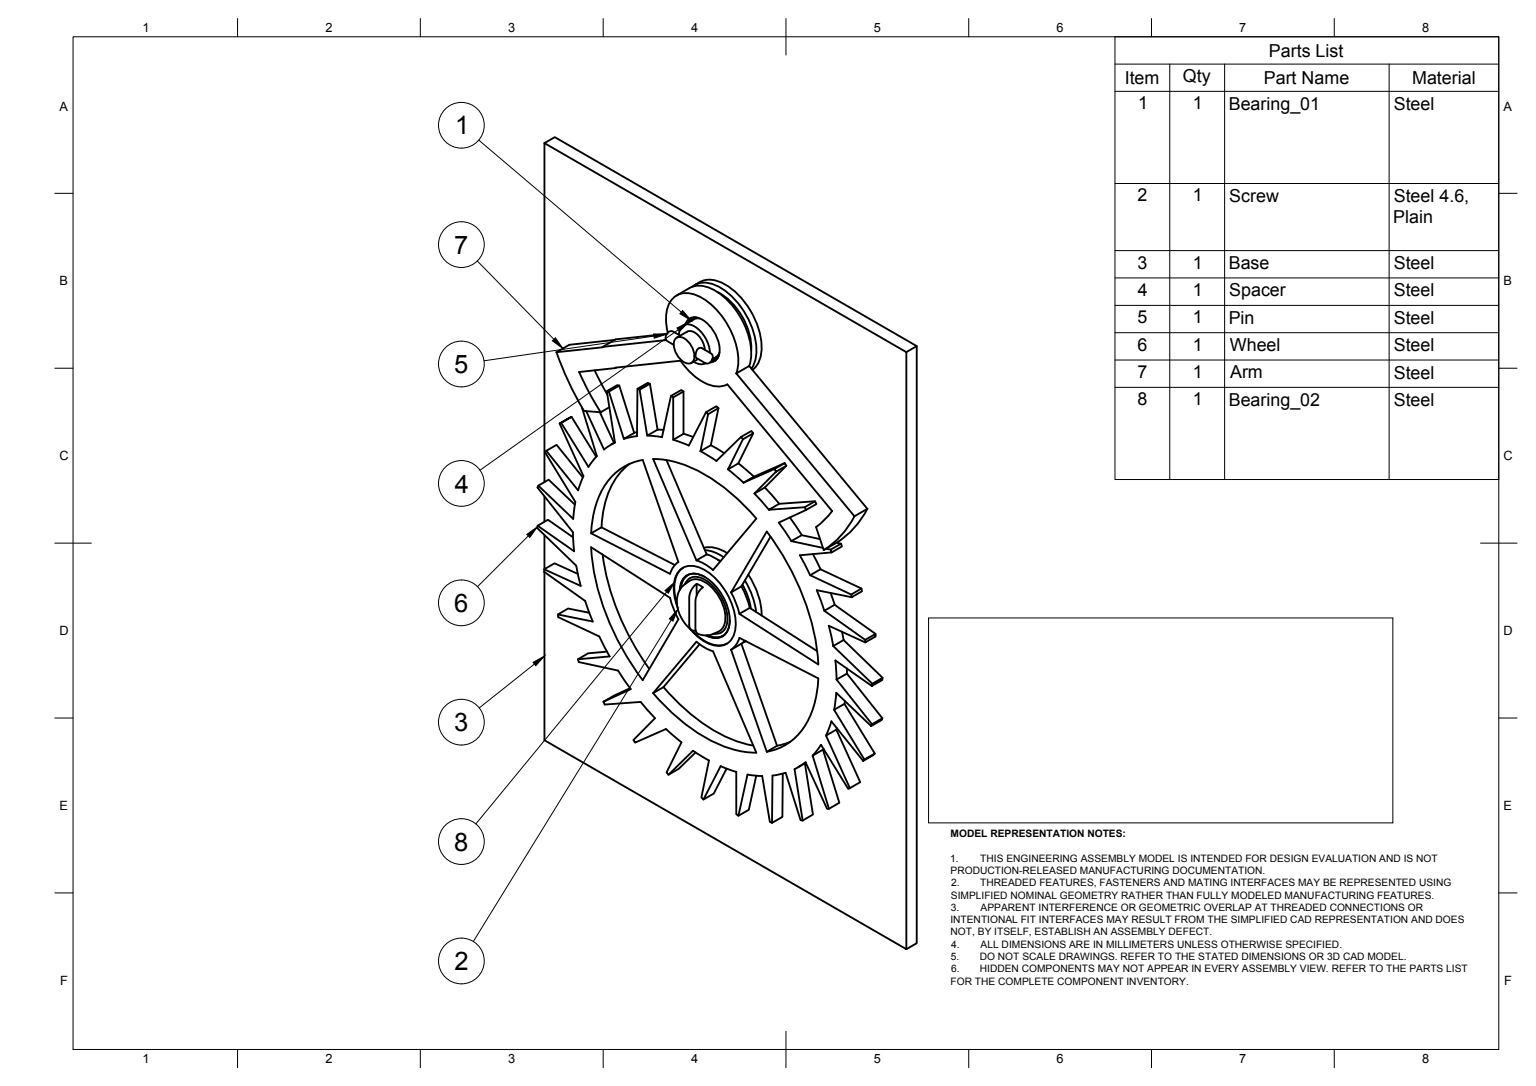
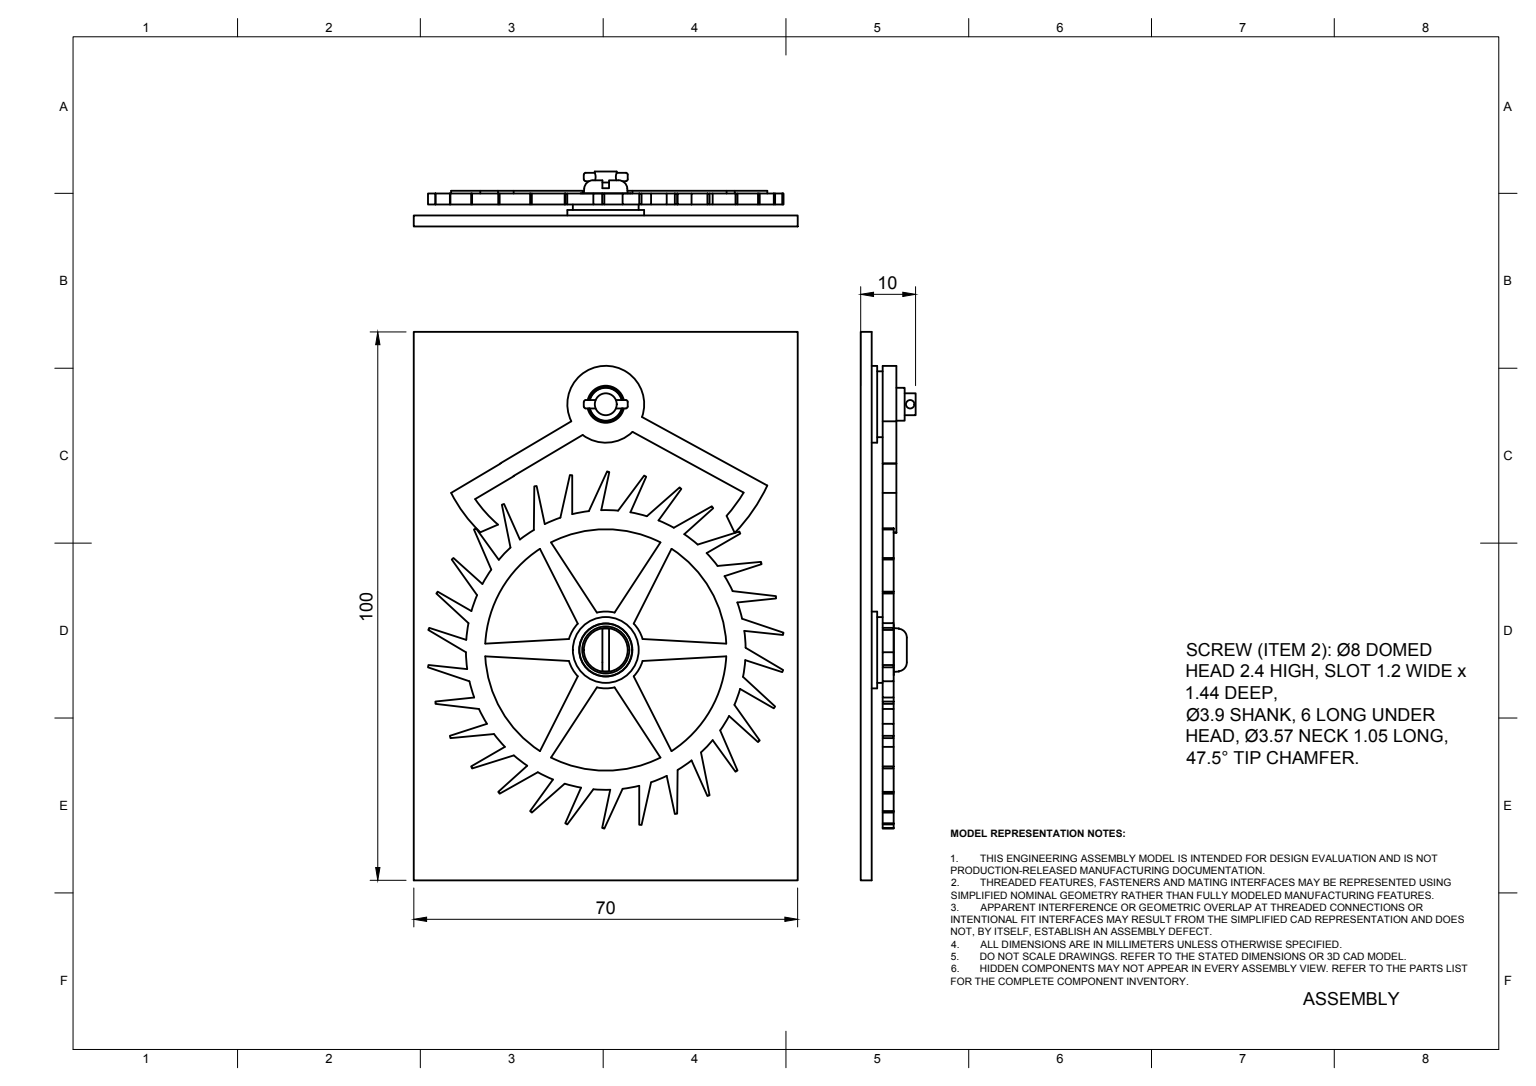
ISO-10303-21;
HEADER;
/* Generated by software containing ST-Developer
 * from STEP Tools, Inc. (www.steptools.com) 
 */

FILE_DESCRIPTION(
/* description */ (''),
/* implementation_level */ '2;1');

FILE_NAME(
/* name */ 'BR-059',
/* time_stamp */ '2026-10-04T15:18:51-07:00',
/* author */ (''),
/* organization */ (''),
/* preprocessor_version */ 'ST-DEVELOPER v20.2',
/* originating_system */ 'Autodesk Translation Framework v15.15.0.0',
/* authorisation */ '');

FILE_SCHEMA (('AUTOMOTIVE_DESIGN { 1 0 10303 214 3 1 1 }'));
ENDSEC;

DATA;
#10=MECHANICAL_DESIGN_GEOMETRIC_PRESENTATION_REPRESENTATION('',(#68,#69,
#70,#71,#72,#73,#74,#75,#76,#77,#78,#79,#80,#81),#9891);
#11=ITEM_DEFINED_TRANSFORMATION($,$,#5720,#6363);
#12=ITEM_DEFINED_TRANSFORMATION($,$,#5863,#6364);
#13=ITEM_DEFINED_TRANSFORMATION($,$,#5890,#6365);
#14=ITEM_DEFINED_TRANSFORMATION($,$,#5919,#6366);
#15=ITEM_DEFINED_TRANSFORMATION($,$,#5928,#6367);
#16=ITEM_DEFINED_TRANSFORMATION($,$,#5948,#6368);
#17=ITEM_DEFINED_TRANSFORMATION($,$,#6182,#6369);
#18=ITEM_DEFINED_TRANSFORMATION($,$,#6220,#6370);
#19=(
REPRESENTATION_RELATIONSHIP($,$,#9923,#9922)
REPRESENTATION_RELATIONSHIP_WITH_TRANSFORMATION(#11)
SHAPE_REPRESENTATION_RELATIONSHIP()
);
#20=(
REPRESENTATION_RELATIONSHIP($,$,#9924,#9922)
REPRESENTATION_RELATIONSHIP_WITH_TRANSFORMATION(#12)
SHAPE_REPRESENTATION_RELATIONSHIP()
);
#21=(
REPRESENTATION_RELATIONSHIP($,$,#9925,#9922)
REPRESENTATION_RELATIONSHIP_WITH_TRANSFORMATION(#13)
SHAPE_REPRESENTATION_RELATIONSHIP()
);
#22=(
REPRESENTATION_RELATIONSHIP($,$,#9926,#9922)
REPRESENTATION_RELATIONSHIP_WITH_TRANSFORMATION(#14)
SHAPE_REPRESENTATION_RELATIONSHIP()
);
#23=(
REPRESENTATION_RELATIONSHIP($,$,#9927,#9922)
REPRESENTATION_RELATIONSHIP_WITH_TRANSFORMATION(#15)
SHAPE_REPRESENTATION_RELATIONSHIP()
);
#24=(
REPRESENTATION_RELATIONSHIP($,$,#9928,#9922)
REPRESENTATION_RELATIONSHIP_WITH_TRANSFORMATION(#16)
SHAPE_REPRESENTATION_RELATIONSHIP()
);
#25=(
REPRESENTATION_RELATIONSHIP($,$,#9929,#9922)
REPRESENTATION_RELATIONSHIP_WITH_TRANSFORMATION(#17)
SHAPE_REPRESENTATION_RELATIONSHIP()
);
#26=(
REPRESENTATION_RELATIONSHIP($,$,#9930,#9922)
REPRESENTATION_RELATIONSHIP_WITH_TRANSFORMATION(#18)
SHAPE_REPRESENTATION_RELATIONSHIP()
);
#27=CONTEXT_DEPENDENT_SHAPE_REPRESENTATION(#19,#9914);
#28=CONTEXT_DEPENDENT_SHAPE_REPRESENTATION(#20,#9915);
#29=CONTEXT_DEPENDENT_SHAPE_REPRESENTATION(#21,#9916);
#30=CONTEXT_DEPENDENT_SHAPE_REPRESENTATION(#22,#9917);
#31=CONTEXT_DEPENDENT_SHAPE_REPRESENTATION(#23,#9918);
#32=CONTEXT_DEPENDENT_SHAPE_REPRESENTATION(#24,#9919);
#33=CONTEXT_DEPENDENT_SHAPE_REPRESENTATION(#25,#9920);
#34=CONTEXT_DEPENDENT_SHAPE_REPRESENTATION(#26,#9921);
#35=NEXT_ASSEMBLY_USAGE_OCCURRENCE('Bearing_01:1','Bearing_01:1',
'Bearing_01:1',#9932,#9933,'Bearing_01:1');
#36=NEXT_ASSEMBLY_USAGE_OCCURRENCE('Screw:1','Screw:1','Screw:1',#9932,
#9934,'Screw:1');
#37=NEXT_ASSEMBLY_USAGE_OCCURRENCE('Base:1','Base:1','Base:1',#9932,#9935,
'Base:1');
#38=NEXT_ASSEMBLY_USAGE_OCCURRENCE('Spacer:1','Spacer:1','Spacer:1',#9932,
#9936,'Spacer:1');
#39=NEXT_ASSEMBLY_USAGE_OCCURRENCE('Pin:1','Pin:1','Pin:1',#9932,#9937,
'Pin:1');
#40=NEXT_ASSEMBLY_USAGE_OCCURRENCE('Wheel:1','Wheel:1','Wheel:1',#9932,
#9938,'Wheel:1');
#41=NEXT_ASSEMBLY_USAGE_OCCURRENCE('Arm:1','Arm:1','Arm:1',#9932,#9939,
'Arm:1');
#42=NEXT_ASSEMBLY_USAGE_OCCURRENCE('Bearing_02:1','Bearing_02:1',
'Bearing_02:1',#9932,#9940,'Bearing_02:1');
#43=B_SPLINE_CURVE_WITH_KNOTS('',3,(#8377,#8378,#8379,#8380,#8381,#8382,
#8383,#8384,#8385,#8386),.UNSPECIFIED.,.F.,.F.,(4,2,2,2,4),(0.015426059292352,
0.0589123817488116,0.11818030974329,0.178151638879277,0.239555012786688),
 .UNSPECIFIED.);
#44=B_SPLINE_CURVE_WITH_KNOTS('',3,(#8390,#8391,#8392,#8393,#8394,#8395,
#8396,#8397,#8398,#8399),.UNSPECIFIED.,.F.,.F.,(4,2,2,2,4),(0.740987738910849,
0.802391112818259,0.862362441954247,0.921630369948725,0.965116692405185),
 .UNSPECIFIED.);
#45=B_SPLINE_CURVE_WITH_KNOTS('',3,(#8404,#8405,#8406,#8407,#8408,#8409,
#8410,#8411,#8412,#8413),.UNSPECIFIED.,.F.,.F.,(4,2,2,2,4),(0.740987738910849,
0.80239111281826,0.862362441954247,0.921630369948725,0.965116692405185),
 .UNSPECIFIED.);
#46=B_SPLINE_CURVE_WITH_KNOTS('',3,(#8417,#8418,#8419,#8420,#8421,#8422,
#8423,#8424,#8425,#8426),.UNSPECIFIED.,.F.,.F.,(4,2,2,2,4),(0.015426059292352,
0.0589123817488117,0.11818030974329,0.178151638879277,0.239555012786688),
 .UNSPECIFIED.);
#47=B_SPLINE_CURVE_WITH_KNOTS('',3,(#8554,#8555,#8556,#8557,#8558,#8559,
#8560,#8561,#8562,#8563,#8564,#8565,#8566,#8567,#8568,#8569,#8570,#8571,
#8572,#8573,#8574,#8575,#8576,#8577,#8578,#8579),.UNSPECIFIED.,.F.,.F.,
(4,2,2,2,2,2,2,2,2,2,2,2,4),(0.,0.0293489859798306,0.0586979719596612,0.0880217900278663,
0.117345608096071,0.146669426164276,0.175993244232481,0.205342230212312,
0.234691216192143,0.264040202171973,0.293389188151804,0.322713006220009,
0.352036824288214),.UNSPECIFIED.);
#48=B_SPLINE_CURVE_WITH_KNOTS('',3,(#8580,#8581,#8582,#8583,#8584,#8585,
#8586,#8587,#8588,#8589),.UNSPECIFIED.,.F.,.F.,(4,2,2,2,4),(0.352036824288214,
0.381360642356419,0.410684460424624,0.440033446404455,0.469382432384286),
 .UNSPECIFIED.);
#49=B_SPLINE_CURVE_WITH_KNOTS('',3,(#8602,#8603,#8604,#8605,#8606,#8607,
#8608,#8609,#8610,#8611),.UNSPECIFIED.,.F.,.F.,(4,2,2,2,4),(0.,0.0293489859798306,
0.0586979719596612,0.0880217900278663,0.117345608096071),.UNSPECIFIED.);
#50=B_SPLINE_CURVE_WITH_KNOTS('',3,(#8613,#8614,#8615,#8616,#8617,#8618,
#8619,#8620,#8621,#8622),.UNSPECIFIED.,.F.,.F.,(4,2,2,2,4),(0.352036824288214,
0.381360642356419,0.410684460424624,0.440033446404455,0.469382432384285),
 .UNSPECIFIED.);
#51=B_SPLINE_CURVE_WITH_KNOTS('',3,(#8623,#8624,#8625,#8626,#8627,#8628,
#8629,#8630,#8631,#8632,#8633,#8634,#8635,#8636,#8637,#8638,#8639,#8640),
 .UNSPECIFIED.,.F.,.F.,(4,2,2,2,2,2,2,2,4),(0.117345608096071,0.146669426164276,
0.175993244232481,0.205342230212312,0.234691216192143,0.264040202171973,
0.293389188151804,0.322713006220009,0.352036824288214),.UNSPECIFIED.);
#52=SHAPE_REPRESENTATION_RELATIONSHIP('SRR','None',#9923,#60);
#53=SHAPE_REPRESENTATION_RELATIONSHIP('SRR','None',#9924,#61);
#54=SHAPE_REPRESENTATION_RELATIONSHIP('SRR','None',#9925,#62);
#55=SHAPE_REPRESENTATION_RELATIONSHIP('SRR','None',#9926,#63);
#56=SHAPE_REPRESENTATION_RELATIONSHIP('SRR','None',#9927,#64);
#57=SHAPE_REPRESENTATION_RELATIONSHIP('SRR','None',#9928,#65);
#58=SHAPE_REPRESENTATION_RELATIONSHIP('SRR','None',#9929,#66);
#59=SHAPE_REPRESENTATION_RELATIONSHIP('SRR','None',#9930,#67);
#60=ADVANCED_BREP_SHAPE_REPRESENTATION('',(#82,#83,#84,#85),#9883);
#61=ADVANCED_BREP_SHAPE_REPRESENTATION('',(#86),#9884);
#62=ADVANCED_BREP_SHAPE_REPRESENTATION('',(#87),#9885);
#63=ADVANCED_BREP_SHAPE_REPRESENTATION('',(#88),#9886);
#64=ADVANCED_BREP_SHAPE_REPRESENTATION('',(#89),#9887);
#65=ADVANCED_BREP_SHAPE_REPRESENTATION('',(#90),#9888);
#66=ADVANCED_BREP_SHAPE_REPRESENTATION('',(#91),#9889);
#67=ADVANCED_BREP_SHAPE_REPRESENTATION('',(#92,#93,#94,#95),#9890);
#68=STYLED_ITEM('',(#9972),#82);
#69=STYLED_ITEM('',(#9972),#83);
#70=STYLED_ITEM('',(#9972),#84);
#71=STYLED_ITEM('',(#9972),#85);
#72=STYLED_ITEM('',(#9973),#86);
#73=STYLED_ITEM('',(#9974),#87);
#74=STYLED_ITEM('',(#9972),#88);
#75=STYLED_ITEM('',(#9972),#89);
#76=STYLED_ITEM('',(#9974),#90);
#77=STYLED_ITEM('',(#9975),#91);
#78=STYLED_ITEM('',(#9972),#92);
#79=STYLED_ITEM('',(#9972),#93);
#80=STYLED_ITEM('',(#9972),#94);
#81=STYLED_ITEM('',(#9972),#95);
#82=MANIFOLD_SOLID_BREP('Body1',#5616);
#83=MANIFOLD_SOLID_BREP('Body2',#5617);
#84=MANIFOLD_SOLID_BREP('Body3',#5618);
#85=MANIFOLD_SOLID_BREP('Body4',#5619);
#86=MANIFOLD_SOLID_BREP('Body1',#5620);
#87=MANIFOLD_SOLID_BREP('Body1',#5621);
#88=MANIFOLD_SOLID_BREP('Body1',#5622);
#89=MANIFOLD_SOLID_BREP('Body1',#5623);
#90=MANIFOLD_SOLID_BREP('Body1',#5624);
#91=MANIFOLD_SOLID_BREP('Body1',#5625);
#92=MANIFOLD_SOLID_BREP('Body1',#5626);
#93=MANIFOLD_SOLID_BREP('Body2',#5627);
#94=MANIFOLD_SOLID_BREP('Body3',#5628);
#95=MANIFOLD_SOLID_BREP('Body4',#5629);
#96=FACE_BOUND('',#746,.T.);
#97=FACE_BOUND('',#748,.T.);
#98=FACE_BOUND('',#750,.T.);
#99=FACE_BOUND('',#752,.T.);
#100=FACE_BOUND('',#764,.T.);
#101=FACE_BOUND('',#766,.T.);
#102=FACE_BOUND('',#768,.T.);
#103=FACE_BOUND('',#770,.T.);
#104=FACE_BOUND('',#784,.T.);
#105=FACE_BOUND('',#786,.T.);
#106=FACE_BOUND('',#788,.T.);
#107=FACE_BOUND('',#790,.T.);
#108=FACE_BOUND('',#792,.T.);
#109=FACE_BOUND('',#806,.T.);
#110=FACE_BOUND('',#808,.T.);
#111=FACE_BOUND('',#810,.T.);
#112=FACE_BOUND('',#812,.T.);
#113=FACE_BOUND('',#814,.T.);
#114=FACE_BOUND('',#825,.T.);
#115=FACE_BOUND('',#834,.T.);
#116=FACE_BOUND('',#836,.T.);
#117=FACE_BOUND('',#837,.T.);
#118=FACE_BOUND('',#841,.T.);
#119=FACE_BOUND('',#843,.T.);
#120=FACE_BOUND('',#849,.T.);
#121=FACE_BOUND('',#850,.T.);
#122=FACE_BOUND('',#852,.T.);
#123=FACE_BOUND('',#856,.T.);
#124=FACE_BOUND('',#858,.T.);
#125=FACE_BOUND('',#867,.T.);
#126=FACE_BOUND('',#1015,.T.);
#127=FACE_BOUND('',#1016,.T.);
#128=FACE_BOUND('',#1017,.T.);
#129=FACE_BOUND('',#1018,.T.);
#130=FACE_BOUND('',#1019,.T.);
#131=FACE_BOUND('',#1020,.T.);
#132=FACE_BOUND('',#1021,.T.);
#133=FACE_BOUND('',#1023,.T.);
#134=FACE_BOUND('',#1024,.T.);
#135=FACE_BOUND('',#1025,.T.);
#136=FACE_BOUND('',#1026,.T.);
#137=FACE_BOUND('',#1027,.T.);
#138=FACE_BOUND('',#1028,.T.);
#139=FACE_BOUND('',#1029,.T.);
#140=FACE_BOUND('',#1032,.T.);
#141=FACE_BOUND('',#1034,.T.);
#142=FACE_BOUND('',#1042,.T.);
#143=FACE_BOUND('',#1063,.T.);
#144=FACE_BOUND('',#1065,.T.);
#145=FACE_BOUND('',#1067,.T.);
#146=FACE_BOUND('',#1069,.T.);
#147=FACE_BOUND('',#1081,.T.);
#148=FACE_BOUND('',#1083,.T.);
#149=FACE_BOUND('',#1085,.T.);
#150=FACE_BOUND('',#1087,.T.);
#151=FACE_BOUND('',#1101,.T.);
#152=FACE_BOUND('',#1103,.T.);
#153=FACE_BOUND('',#1105,.T.);
#154=FACE_BOUND('',#1107,.T.);
#155=FACE_BOUND('',#1109,.T.);
#156=FACE_BOUND('',#1123,.T.);
#157=FACE_BOUND('',#1125,.T.);
#158=FACE_BOUND('',#1127,.T.);
#159=FACE_BOUND('',#1129,.T.);
#160=FACE_BOUND('',#1131,.T.);
#161=PLANE('',#5744);
#162=PLANE('',#5745);
#163=PLANE('',#5746);
#164=PLANE('',#5747);
#165=PLANE('',#5777);
#166=PLANE('',#5778);
#167=PLANE('',#5779);
#168=PLANE('',#5780);
#169=PLANE('',#5817);
#170=PLANE('',#5818);
#171=PLANE('',#5819);
#172=PLANE('',#5820);
#173=PLANE('',#5821);
#174=PLANE('',#5858);
#175=PLANE('',#5859);
#176=PLANE('',#5860);
#177=PLANE('',#5861);
#178=PLANE('',#5862);
#179=PLANE('',#5867);
#180=PLANE('',#5868);
#181=PLANE('',#5869);
#182=PLANE('',#5873);
#183=PLANE('',#5875);
#184=PLANE('',#5882);
#185=PLANE('',#5883);
#186=PLANE('',#5903);
#187=PLANE('',#5904);
#188=PLANE('',#5911);
#189=PLANE('',#5912);
#190=PLANE('',#5913);
#191=PLANE('',#5914);
#192=PLANE('',#5915);
#193=PLANE('',#5916);
#194=PLANE('',#5917);
#195=PLANE('',#5918);
#196=PLANE('',#5926);
#197=PLANE('',#5927);
#198=PLANE('',#5935);
#199=PLANE('',#5942);
#200=PLANE('',#5943);
#201=PLANE('',#5947);
#202=PLANE('',#5949);
#203=PLANE('',#5950);
#204=PLANE('',#5951);
#205=PLANE('',#5958);
#206=PLANE('',#5959);
#207=PLANE('',#5960);
#208=PLANE('',#5964);
#209=PLANE('',#5965);
#210=PLANE('',#5966);
#211=PLANE('',#5970);
#212=PLANE('',#5971);
#213=PLANE('',#5972);
#214=PLANE('',#5976);
#215=PLANE('',#5977);
#216=PLANE('',#5978);
#217=PLANE('',#5982);
#218=PLANE('',#5983);
#219=PLANE('',#5984);
#220=PLANE('',#5991);
#221=PLANE('',#5992);
#222=PLANE('',#5993);
#223=PLANE('',#5994);
#224=PLANE('',#5995);
#225=PLANE('',#5996);
#226=PLANE('',#6000);
#227=PLANE('',#6001);
#228=PLANE('',#6002);
#229=PLANE('',#6009);
#230=PLANE('',#6010);
#231=PLANE('',#6011);
#232=PLANE('',#6018);
#233=PLANE('',#6019);
#234=PLANE('',#6020);
#235=PLANE('',#6021);
#236=PLANE('',#6022);
#237=PLANE('',#6023);
#238=PLANE('',#6024);
#239=PLANE('',#6025);
#240=PLANE('',#6026);
#241=PLANE('',#6030);
#242=PLANE('',#6031);
#243=PLANE('',#6032);
#244=PLANE('',#6036);
#245=PLANE('',#6037);
#246=PLANE('',#6038);
#247=PLANE('',#6045);
#248=PLANE('',#6046);
#249=PLANE('',#6047);
#250=PLANE('',#6051);
#251=PLANE('',#6052);
#252=PLANE('',#6053);
#253=PLANE('',#6057);
#254=PLANE('',#6058);
#255=PLANE('',#6059);
#256=PLANE('',#6060);
#257=PLANE('',#6061);
#258=PLANE('',#6062);
#259=PLANE('',#6069);
#260=PLANE('',#6070);
#261=PLANE('',#6071);
#262=PLANE('',#6072);
#263=PLANE('',#6073);
#264=PLANE('',#6074);
#265=PLANE('',#6081);
#266=PLANE('',#6082);
#267=PLANE('',#6083);
#268=PLANE('',#6084);
#269=PLANE('',#6085);
#270=PLANE('',#6086);
#271=PLANE('',#6093);
#272=PLANE('',#6094);
#273=PLANE('',#6095);
#274=PLANE('',#6099);
#275=PLANE('',#6100);
#276=PLANE('',#6101);
#277=PLANE('',#6105);
#278=PLANE('',#6106);
#279=PLANE('',#6107);
#280=PLANE('',#6111);
#281=PLANE('',#6112);
#282=PLANE('',#6113);
#283=PLANE('',#6120);
#284=PLANE('',#6121);
#285=PLANE('',#6122);
#286=PLANE('',#6123);
#287=PLANE('',#6124);
#288=PLANE('',#6125);
#289=PLANE('',#6126);
#290=PLANE('',#6127);
#291=PLANE('',#6128);
#292=PLANE('',#6129);
#293=PLANE('',#6130);
#294=PLANE('',#6143);
#295=PLANE('',#6144);
#296=PLANE('',#6151);
#297=PLANE('',#6152);
#298=PLANE('',#6159);
#299=PLANE('',#6160);
#300=PLANE('',#6167);
#301=PLANE('',#6168);
#302=PLANE('',#6175);
#303=PLANE('',#6176);
#304=PLANE('',#6180);
#305=PLANE('',#6181);
#306=PLANE('',#6186);
#307=PLANE('',#6188);
#308=PLANE('',#6195);
#309=PLANE('',#6198);
#310=PLANE('',#6201);
#311=PLANE('',#6202);
#312=PLANE('',#6203);
#313=PLANE('',#6209);
#314=PLANE('',#6210);
#315=PLANE('',#6213);
#316=PLANE('',#6215);
#317=PLANE('',#6217);
#318=PLANE('',#6219);
#319=PLANE('',#6244);
#320=PLANE('',#6245);
#321=PLANE('',#6246);
#322=PLANE('',#6247);
#323=PLANE('',#6277);
#324=PLANE('',#6278);
#325=PLANE('',#6279);
#326=PLANE('',#6280);
#327=PLANE('',#6317);
#328=PLANE('',#6318);
#329=PLANE('',#6319);
#330=PLANE('',#6320);
#331=PLANE('',#6321);
#332=PLANE('',#6358);
#333=PLANE('',#6359);
#334=PLANE('',#6360);
#335=PLANE('',#6361);
#336=PLANE('',#6362);
#337=TOROIDAL_SURFACE('',#5733,5.8,0.2);
#338=TOROIDAL_SURFACE('',#5739,5.8,0.2);
#339=TOROIDAL_SURFACE('',#5754,3.25741379310345,0.138976293103448);
#340=TOROIDAL_SURFACE('',#5760,3.25741379310345,0.138976293103448);
#341=TOROIDAL_SURFACE('',#5768,2.2,0.2);
#342=TOROIDAL_SURFACE('',#5774,2.2,0.2);
#343=TOROIDAL_SURFACE('',#5784,4.14313829631318,0.0900000000000005);
#344=TOROIDAL_SURFACE('',#5790,4.38370090847553,0.0200000000000002);
#345=TOROIDAL_SURFACE('',#5793,4.58,0.119999999999999);
#346=TOROIDAL_SURFACE('',#5799,4.51071796769724,0.12);
#347=TOROIDAL_SURFACE('',#5802,4.51071796769724,0.22);
#348=TOROIDAL_SURFACE('',#5808,4.58,0.219999999999999);
#349=TOROIDAL_SURFACE('',#5811,4.38370090847553,0.12);
#350=TOROIDAL_SURFACE('',#5825,4.14313829631318,0.0900000000000005);
#351=TOROIDAL_SURFACE('',#5831,4.38370090847553,0.0200000000000002);
#352=TOROIDAL_SURFACE('',#5834,4.58,0.119999999999999);
#353=TOROIDAL_SURFACE('',#5840,4.51071796769724,0.12);
#354=TOROIDAL_SURFACE('',#5843,4.51071796769724,0.22);
#355=TOROIDAL_SURFACE('',#5849,4.58,0.219999999999999);
#356=TOROIDAL_SURFACE('',#5852,4.38370090847553,0.12);
#357=TOROIDAL_SURFACE('',#5877,2.32389732910985,1.6);
#358=TOROIDAL_SURFACE('',#5929,0.420000000000005,0.35);
#359=TOROIDAL_SURFACE('',#5936,0.420000000000005,0.35);
#360=TOROIDAL_SURFACE('',#6233,5.8,0.2);
#361=TOROIDAL_SURFACE('',#6239,5.8,0.2);
#362=TOROIDAL_SURFACE('',#6254,3.25741379310345,0.138976293103448);
#363=TOROIDAL_SURFACE('',#6260,3.25741379310345,0.138976293103448);
#364=TOROIDAL_SURFACE('',#6268,2.2,0.2);
#365=TOROIDAL_SURFACE('',#6274,2.2,0.2);
#366=TOROIDAL_SURFACE('',#6284,4.14313829631318,0.0900000000000005);
#367=TOROIDAL_SURFACE('',#6290,4.38370090847553,0.0200000000000002);
#368=TOROIDAL_SURFACE('',#6293,4.58,0.119999999999999);
#369=TOROIDAL_SURFACE('',#6299,4.51071796769724,0.12);
#370=TOROIDAL_SURFACE('',#6302,4.51071796769724,0.22);
#371=TOROIDAL_SURFACE('',#6308,4.58,0.219999999999999);
#372=TOROIDAL_SURFACE('',#6311,4.38370090847553,0.12);
#373=TOROIDAL_SURFACE('',#6325,4.14313829631318,0.0900000000000005);
#374=TOROIDAL_SURFACE('',#6331,4.38370090847553,0.0200000000000002);
#375=TOROIDAL_SURFACE('',#6334,4.58,0.119999999999999);
#376=TOROIDAL_SURFACE('',#6340,4.51071796769724,0.12);
#377=TOROIDAL_SURFACE('',#6343,4.51071796769724,0.22);
#378=TOROIDAL_SURFACE('',#6349,4.58,0.219999999999999);
#379=TOROIDAL_SURFACE('',#6352,4.38370090847553,0.12);
#380=CONICAL_SURFACE('',#5731,4.8,0.785398163397444);
#381=CONICAL_SURFACE('',#5742,4.845,0.785398163397444);
#382=CONICAL_SURFACE('',#5748,3.1184375,0.785398163397448);
#383=CONICAL_SURFACE('',#5766,3.0734375,0.785398163397448);
#384=CONICAL_SURFACE('',#5788,4.36638040039984,0.52359877559829);
#385=CONICAL_SURFACE('',#5797,4.57071796769724,1.04719755119659);
#386=CONICAL_SURFACE('',#5806,4.62071796769724,1.04719755119659);
#387=CONICAL_SURFACE('',#5815,4.27977786002139,0.52359877559829);
#388=CONICAL_SURFACE('',#5829,4.36638040039984,0.52359877559829);
#389=CONICAL_SURFACE('',#5838,4.57071796769724,1.04719755119659);
#390=CONICAL_SURFACE('',#5847,4.62071796769724,1.04719755119659);
#391=CONICAL_SURFACE('',#5856,4.27977786002139,0.52359877559829);
#392=CONICAL_SURFACE('',#5864,1.8052925,0.829871117430571);
#393=CONICAL_SURFACE('',#5880,3.8950136037689,0.0872664625996596);
#394=CONICAL_SURFACE('',#5887,1.89262500000135,0.523598775596927);
#395=CONICAL_SURFACE('',#6231,4.8,0.785398163397444);
#396=CONICAL_SURFACE('',#6242,4.845,0.785398163397444);
#397=CONICAL_SURFACE('',#6248,3.1184375,0.785398163397448);
#398=CONICAL_SURFACE('',#6266,3.0734375,0.785398163397448);
#399=CONICAL_SURFACE('',#6288,4.36638040039984,0.52359877559829);
#400=CONICAL_SURFACE('',#6297,4.57071796769724,1.04719755119659);
#401=CONICAL_SURFACE('',#6306,4.62071796769724,1.04719755119659);
#402=CONICAL_SURFACE('',#6315,4.27977786002139,0.52359877559829);
#403=CONICAL_SURFACE('',#6329,4.36638040039984,0.52359877559829);
#404=CONICAL_SURFACE('',#6338,4.57071796769724,1.04719755119659);
#405=CONICAL_SURFACE('',#6347,4.62071796769724,1.04719755119659);
#406=CONICAL_SURFACE('',#6356,4.27977786002139,0.52359877559829);
#407=FACE_OUTER_BOUND('',#737,.T.);
#408=FACE_OUTER_BOUND('',#738,.T.);
#409=FACE_OUTER_BOUND('',#739,.T.);
#410=FACE_OUTER_BOUND('',#740,.T.);
#411=FACE_OUTER_BOUND('',#741,.T.);
#412=FACE_OUTER_BOUND('',#742,.T.);
#413=FACE_OUTER_BOUND('',#743,.T.);
#414=FACE_OUTER_BOUND('',#744,.T.);
#415=FACE_OUTER_BOUND('',#745,.T.);
#416=FACE_OUTER_BOUND('',#747,.T.);
#417=FACE_OUTER_BOUND('',#749,.T.);
#418=FACE_OUTER_BOUND('',#751,.T.);
#419=FACE_OUTER_BOUND('',#753,.T.);
#420=FACE_OUTER_BOUND('',#754,.T.);
#421=FACE_OUTER_BOUND('',#755,.T.);
#422=FACE_OUTER_BOUND('',#756,.T.);
#423=FACE_OUTER_BOUND('',#757,.T.);
#424=FACE_OUTER_BOUND('',#758,.T.);
#425=FACE_OUTER_BOUND('',#759,.T.);
#426=FACE_OUTER_BOUND('',#760,.T.);
#427=FACE_OUTER_BOUND('',#761,.T.);
#428=FACE_OUTER_BOUND('',#762,.T.);
#429=FACE_OUTER_BOUND('',#763,.T.);
#430=FACE_OUTER_BOUND('',#765,.T.);
#431=FACE_OUTER_BOUND('',#767,.T.);
#432=FACE_OUTER_BOUND('',#769,.T.);
#433=FACE_OUTER_BOUND('',#771,.T.);
#434=FACE_OUTER_BOUND('',#772,.T.);
#435=FACE_OUTER_BOUND('',#773,.T.);
#436=FACE_OUTER_BOUND('',#774,.T.);
#437=FACE_OUTER_BOUND('',#775,.T.);
#438=FACE_OUTER_BOUND('',#776,.T.);
#439=FACE_OUTER_BOUND('',#777,.T.);
#440=FACE_OUTER_BOUND('',#778,.T.);
#441=FACE_OUTER_BOUND('',#779,.T.);
#442=FACE_OUTER_BOUND('',#780,.T.);
#443=FACE_OUTER_BOUND('',#781,.T.);
#444=FACE_OUTER_BOUND('',#782,.T.);
#445=FACE_OUTER_BOUND('',#783,.T.);
#446=FACE_OUTER_BOUND('',#785,.T.);
#447=FACE_OUTER_BOUND('',#787,.T.);
#448=FACE_OUTER_BOUND('',#789,.T.);
#449=FACE_OUTER_BOUND('',#791,.T.);
#450=FACE_OUTER_BOUND('',#793,.T.);
#451=FACE_OUTER_BOUND('',#794,.T.);
#452=FACE_OUTER_BOUND('',#795,.T.);
#453=FACE_OUTER_BOUND('',#796,.T.);
#454=FACE_OUTER_BOUND('',#797,.T.);
#455=FACE_OUTER_BOUND('',#798,.T.);
#456=FACE_OUTER_BOUND('',#799,.T.);
#457=FACE_OUTER_BOUND('',#800,.T.);
#458=FACE_OUTER_BOUND('',#801,.T.);
#459=FACE_OUTER_BOUND('',#802,.T.);
#460=FACE_OUTER_BOUND('',#803,.T.);
#461=FACE_OUTER_BOUND('',#804,.T.);
#462=FACE_OUTER_BOUND('',#805,.T.);
#463=FACE_OUTER_BOUND('',#807,.T.);
#464=FACE_OUTER_BOUND('',#809,.T.);
#465=FACE_OUTER_BOUND('',#811,.T.);
#466=FACE_OUTER_BOUND('',#813,.T.);
#467=FACE_OUTER_BOUND('',#815,.T.);
#468=FACE_OUTER_BOUND('',#816,.T.);
#469=FACE_OUTER_BOUND('',#817,.T.);
#470=FACE_OUTER_BOUND('',#818,.T.);
#471=FACE_OUTER_BOUND('',#819,.T.);
#472=FACE_OUTER_BOUND('',#820,.T.);
#473=FACE_OUTER_BOUND('',#821,.T.);
#474=FACE_OUTER_BOUND('',#822,.T.);
#475=FACE_OUTER_BOUND('',#823,.T.);
#476=FACE_OUTER_BOUND('',#824,.T.);
#477=FACE_OUTER_BOUND('',#826,.T.);
#478=FACE_OUTER_BOUND('',#827,.T.);
#479=FACE_OUTER_BOUND('',#828,.T.);
#480=FACE_OUTER_BOUND('',#829,.T.);
#481=FACE_OUTER_BOUND('',#830,.T.);
#482=FACE_OUTER_BOUND('',#831,.T.);
#483=FACE_OUTER_BOUND('',#832,.T.);
#484=FACE_OUTER_BOUND('',#833,.T.);
#485=FACE_OUTER_BOUND('',#835,.T.);
#486=FACE_OUTER_BOUND('',#838,.T.);
#487=FACE_OUTER_BOUND('',#839,.T.);
#488=FACE_OUTER_BOUND('',#840,.T.);
#489=FACE_OUTER_BOUND('',#842,.T.);
#490=FACE_OUTER_BOUND('',#844,.T.);
#491=FACE_OUTER_BOUND('',#845,.T.);
#492=FACE_OUTER_BOUND('',#846,.T.);
#493=FACE_OUTER_BOUND('',#847,.T.);
#494=FACE_OUTER_BOUND('',#848,.T.);
#495=FACE_OUTER_BOUND('',#851,.T.);
#496=FACE_OUTER_BOUND('',#853,.T.);
#497=FACE_OUTER_BOUND('',#854,.T.);
#498=FACE_OUTER_BOUND('',#855,.T.);
#499=FACE_OUTER_BOUND('',#857,.T.);
#500=FACE_OUTER_BOUND('',#859,.T.);
#501=FACE_OUTER_BOUND('',#860,.T.);
#502=FACE_OUTER_BOUND('',#861,.T.);
#503=FACE_OUTER_BOUND('',#862,.T.);
#504=FACE_OUTER_BOUND('',#863,.T.);
#505=FACE_OUTER_BOUND('',#864,.T.);
#506=FACE_OUTER_BOUND('',#865,.T.);
#507=FACE_OUTER_BOUND('',#866,.T.);
#508=FACE_OUTER_BOUND('',#868,.T.);
#509=FACE_OUTER_BOUND('',#869,.T.);
#510=FACE_OUTER_BOUND('',#870,.T.);
#511=FACE_OUTER_BOUND('',#871,.T.);
#512=FACE_OUTER_BOUND('',#872,.T.);
#513=FACE_OUTER_BOUND('',#873,.T.);
#514=FACE_OUTER_BOUND('',#874,.T.);
#515=FACE_OUTER_BOUND('',#875,.T.);
#516=FACE_OUTER_BOUND('',#876,.T.);
#517=FACE_OUTER_BOUND('',#877,.T.);
#518=FACE_OUTER_BOUND('',#878,.T.);
#519=FACE_OUTER_BOUND('',#879,.T.);
#520=FACE_OUTER_BOUND('',#880,.T.);
#521=FACE_OUTER_BOUND('',#881,.T.);
#522=FACE_OUTER_BOUND('',#882,.T.);
#523=FACE_OUTER_BOUND('',#883,.T.);
#524=FACE_OUTER_BOUND('',#884,.T.);
#525=FACE_OUTER_BOUND('',#885,.T.);
#526=FACE_OUTER_BOUND('',#886,.T.);
#527=FACE_OUTER_BOUND('',#887,.T.);
#528=FACE_OUTER_BOUND('',#888,.T.);
#529=FACE_OUTER_BOUND('',#889,.T.);
#530=FACE_OUTER_BOUND('',#890,.T.);
#531=FACE_OUTER_BOUND('',#891,.T.);
#532=FACE_OUTER_BOUND('',#892,.T.);
#533=FACE_OUTER_BOUND('',#893,.T.);
#534=FACE_OUTER_BOUND('',#894,.T.);
#535=FACE_OUTER_BOUND('',#895,.T.);
#536=FACE_OUTER_BOUND('',#896,.T.);
#537=FACE_OUTER_BOUND('',#897,.T.);
#538=FACE_OUTER_BOUND('',#898,.T.);
#539=FACE_OUTER_BOUND('',#899,.T.);
#540=FACE_OUTER_BOUND('',#900,.T.);
#541=FACE_OUTER_BOUND('',#901,.T.);
#542=FACE_OUTER_BOUND('',#902,.T.);
#543=FACE_OUTER_BOUND('',#903,.T.);
#544=FACE_OUTER_BOUND('',#904,.T.);
#545=FACE_OUTER_BOUND('',#905,.T.);
#546=FACE_OUTER_BOUND('',#906,.T.);
#547=FACE_OUTER_BOUND('',#907,.T.);
#548=FACE_OUTER_BOUND('',#908,.T.);
#549=FACE_OUTER_BOUND('',#909,.T.);
#550=FACE_OUTER_BOUND('',#910,.T.);
#551=FACE_OUTER_BOUND('',#911,.T.);
#552=FACE_OUTER_BOUND('',#912,.T.);
#553=FACE_OUTER_BOUND('',#913,.T.);
#554=FACE_OUTER_BOUND('',#914,.T.);
#555=FACE_OUTER_BOUND('',#915,.T.);
#556=FACE_OUTER_BOUND('',#916,.T.);
#557=FACE_OUTER_BOUND('',#917,.T.);
#558=FACE_OUTER_BOUND('',#918,.T.);
#559=FACE_OUTER_BOUND('',#919,.T.);
#560=FACE_OUTER_BOUND('',#920,.T.);
#561=FACE_OUTER_BOUND('',#921,.T.);
#562=FACE_OUTER_BOUND('',#922,.T.);
#563=FACE_OUTER_BOUND('',#923,.T.);
#564=FACE_OUTER_BOUND('',#924,.T.);
#565=FACE_OUTER_BOUND('',#925,.T.);
#566=FACE_OUTER_BOUND('',#926,.T.);
#567=FACE_OUTER_BOUND('',#927,.T.);
#568=FACE_OUTER_BOUND('',#928,.T.);
#569=FACE_OUTER_BOUND('',#929,.T.);
#570=FACE_OUTER_BOUND('',#930,.T.);
#571=FACE_OUTER_BOUND('',#931,.T.);
#572=FACE_OUTER_BOUND('',#932,.T.);
#573=FACE_OUTER_BOUND('',#933,.T.);
#574=FACE_OUTER_BOUND('',#934,.T.);
#575=FACE_OUTER_BOUND('',#935,.T.);
#576=FACE_OUTER_BOUND('',#936,.T.);
#577=FACE_OUTER_BOUND('',#937,.T.);
#578=FACE_OUTER_BOUND('',#938,.T.);
#579=FACE_OUTER_BOUND('',#939,.T.);
#580=FACE_OUTER_BOUND('',#940,.T.);
#581=FACE_OUTER_BOUND('',#941,.T.);
#582=FACE_OUTER_BOUND('',#942,.T.);
#583=FACE_OUTER_BOUND('',#943,.T.);
#584=FACE_OUTER_BOUND('',#944,.T.);
#585=FACE_OUTER_BOUND('',#945,.T.);
#586=FACE_OUTER_BOUND('',#946,.T.);
#587=FACE_OUTER_BOUND('',#947,.T.);
#588=FACE_OUTER_BOUND('',#948,.T.);
#589=FACE_OUTER_BOUND('',#949,.T.);
#590=FACE_OUTER_BOUND('',#950,.T.);
#591=FACE_OUTER_BOUND('',#951,.T.);
#592=FACE_OUTER_BOUND('',#952,.T.);
#593=FACE_OUTER_BOUND('',#953,.T.);
#594=FACE_OUTER_BOUND('',#954,.T.);
#595=FACE_OUTER_BOUND('',#955,.T.);
#596=FACE_OUTER_BOUND('',#956,.T.);
#597=FACE_OUTER_BOUND('',#957,.T.);
#598=FACE_OUTER_BOUND('',#958,.T.);
#599=FACE_OUTER_BOUND('',#959,.T.);
#600=FACE_OUTER_BOUND('',#960,.T.);
#601=FACE_OUTER_BOUND('',#961,.T.);
#602=FACE_OUTER_BOUND('',#962,.T.);
#603=FACE_OUTER_BOUND('',#963,.T.);
#604=FACE_OUTER_BOUND('',#964,.T.);
#605=FACE_OUTER_BOUND('',#965,.T.);
#606=FACE_OUTER_BOUND('',#966,.T.);
#607=FACE_OUTER_BOUND('',#967,.T.);
#608=FACE_OUTER_BOUND('',#968,.T.);
#609=FACE_OUTER_BOUND('',#969,.T.);
#610=FACE_OUTER_BOUND('',#970,.T.);
#611=FACE_OUTER_BOUND('',#971,.T.);
#612=FACE_OUTER_BOUND('',#972,.T.);
#613=FACE_OUTER_BOUND('',#973,.T.);
#614=FACE_OUTER_BOUND('',#974,.T.);
#615=FACE_OUTER_BOUND('',#975,.T.);
#616=FACE_OUTER_BOUND('',#976,.T.);
#617=FACE_OUTER_BOUND('',#977,.T.);
#618=FACE_OUTER_BOUND('',#978,.T.);
#619=FACE_OUTER_BOUND('',#979,.T.);
#620=FACE_OUTER_BOUND('',#980,.T.);
#621=FACE_OUTER_BOUND('',#981,.T.);
#622=FACE_OUTER_BOUND('',#982,.T.);
#623=FACE_OUTER_BOUND('',#983,.T.);
#624=FACE_OUTER_BOUND('',#984,.T.);
#625=FACE_OUTER_BOUND('',#985,.T.);
#626=FACE_OUTER_BOUND('',#986,.T.);
#627=FACE_OUTER_BOUND('',#987,.T.);
#628=FACE_OUTER_BOUND('',#988,.T.);
#629=FACE_OUTER_BOUND('',#989,.T.);
#630=FACE_OUTER_BOUND('',#990,.T.);
#631=FACE_OUTER_BOUND('',#991,.T.);
#632=FACE_OUTER_BOUND('',#992,.T.);
#633=FACE_OUTER_BOUND('',#993,.T.);
#634=FACE_OUTER_BOUND('',#994,.T.);
#635=FACE_OUTER_BOUND('',#995,.T.);
#636=FACE_OUTER_BOUND('',#996,.T.);
#637=FACE_OUTER_BOUND('',#997,.T.);
#638=FACE_OUTER_BOUND('',#998,.T.);
#639=FACE_OUTER_BOUND('',#999,.T.);
#640=FACE_OUTER_BOUND('',#1000,.T.);
#641=FACE_OUTER_BOUND('',#1001,.T.);
#642=FACE_OUTER_BOUND('',#1002,.T.);
#643=FACE_OUTER_BOUND('',#1003,.T.);
#644=FACE_OUTER_BOUND('',#1004,.T.);
#645=FACE_OUTER_BOUND('',#1005,.T.);
#646=FACE_OUTER_BOUND('',#1006,.T.);
#647=FACE_OUTER_BOUND('',#1007,.T.);
#648=FACE_OUTER_BOUND('',#1008,.T.);
#649=FACE_OUTER_BOUND('',#1009,.T.);
#650=FACE_OUTER_BOUND('',#1010,.T.);
#651=FACE_OUTER_BOUND('',#1011,.T.);
#652=FACE_OUTER_BOUND('',#1012,.T.);
#653=FACE_OUTER_BOUND('',#1013,.T.);
#654=FACE_OUTER_BOUND('',#1014,.T.);
#655=FACE_OUTER_BOUND('',#1022,.T.);
#656=FACE_OUTER_BOUND('',#1030,.T.);
#657=FACE_OUTER_BOUND('',#1031,.T.);
#658=FACE_OUTER_BOUND('',#1033,.T.);
#659=FACE_OUTER_BOUND('',#1035,.T.);
#660=FACE_OUTER_BOUND('',#1036,.T.);
#661=FACE_OUTER_BOUND('',#1037,.T.);
#662=FACE_OUTER_BOUND('',#1038,.T.);
#663=FACE_OUTER_BOUND('',#1039,.T.);
#664=FACE_OUTER_BOUND('',#1040,.T.);
#665=FACE_OUTER_BOUND('',#1041,.T.);
#666=FACE_OUTER_BOUND('',#1043,.T.);
#667=FACE_OUTER_BOUND('',#1044,.T.);
#668=FACE_OUTER_BOUND('',#1045,.T.);
#669=FACE_OUTER_BOUND('',#1046,.T.);
#670=FACE_OUTER_BOUND('',#1047,.T.);
#671=FACE_OUTER_BOUND('',#1048,.T.);
#672=FACE_OUTER_BOUND('',#1049,.T.);
#673=FACE_OUTER_BOUND('',#1050,.T.);
#674=FACE_OUTER_BOUND('',#1051,.T.);
#675=FACE_OUTER_BOUND('',#1052,.T.);
#676=FACE_OUTER_BOUND('',#1053,.T.);
#677=FACE_OUTER_BOUND('',#1054,.T.);
#678=FACE_OUTER_BOUND('',#1055,.T.);
#679=FACE_OUTER_BOUND('',#1056,.T.);
#680=FACE_OUTER_BOUND('',#1057,.T.);
#681=FACE_OUTER_BOUND('',#1058,.T.);
#682=FACE_OUTER_BOUND('',#1059,.T.);
#683=FACE_OUTER_BOUND('',#1060,.T.);
#684=FACE_OUTER_BOUND('',#1061,.T.);
#685=FACE_OUTER_BOUND('',#1062,.T.);
#686=FACE_OUTER_BOUND('',#1064,.T.);
#687=FACE_OUTER_BOUND('',#1066,.T.);
#688=FACE_OUTER_BOUND('',#1068,.T.);
#689=FACE_OUTER_BOUND('',#1070,.T.);
#690=FACE_OUTER_BOUND('',#1071,.T.);
#691=FACE_OUTER_BOUND('',#1072,.T.);
#692=FACE_OUTER_BOUND('',#1073,.T.);
#693=FACE_OUTER_BOUND('',#1074,.T.);
#694=FACE_OUTER_BOUND('',#1075,.T.);
#695=FACE_OUTER_BOUND('',#1076,.T.);
#696=FACE_OUTER_BOUND('',#1077,.T.);
#697=FACE_OUTER_BOUND('',#1078,.T.);
#698=FACE_OUTER_BOUND('',#1079,.T.);
#699=FACE_OUTER_BOUND('',#1080,.T.);
#700=FACE_OUTER_BOUND('',#1082,.T.);
#701=FACE_OUTER_BOUND('',#1084,.T.);
#702=FACE_OUTER_BOUND('',#1086,.T.);
#703=FACE_OUTER_BOUND('',#1088,.T.);
#704=FACE_OUTER_BOUND('',#1089,.T.);
#705=FACE_OUTER_BOUND('',#1090,.T.);
#706=FACE_OUTER_BOUND('',#1091,.T.);
#707=FACE_OUTER_BOUND('',#1092,.T.);
#708=FACE_OUTER_BOUND('',#1093,.T.);
#709=FACE_OUTER_BOUND('',#1094,.T.);
#710=FACE_OUTER_BOUND('',#1095,.T.);
#711=FACE_OUTER_BOUND('',#1096,.T.);
#712=FACE_OUTER_BOUND('',#1097,.T.);
#713=FACE_OUTER_BOUND('',#1098,.T.);
#714=FACE_OUTER_BOUND('',#1099,.T.);
#715=FACE_OUTER_BOUND('',#1100,.T.);
#716=FACE_OUTER_BOUND('',#1102,.T.);
#717=FACE_OUTER_BOUND('',#1104,.T.);
#718=FACE_OUTER_BOUND('',#1106,.T.);
#719=FACE_OUTER_BOUND('',#1108,.T.);
#720=FACE_OUTER_BOUND('',#1110,.T.);
#721=FACE_OUTER_BOUND('',#1111,.T.);
#722=FACE_OUTER_BOUND('',#1112,.T.);
#723=FACE_OUTER_BOUND('',#1113,.T.);
#724=FACE_OUTER_BOUND('',#1114,.T.);
#725=FACE_OUTER_BOUND('',#1115,.T.);
#726=FACE_OUTER_BOUND('',#1116,.T.);
#727=FACE_OUTER_BOUND('',#1117,.T.);
#728=FACE_OUTER_BOUND('',#1118,.T.);
#729=FACE_OUTER_BOUND('',#1119,.T.);
#730=FACE_OUTER_BOUND('',#1120,.T.);
#731=FACE_OUTER_BOUND('',#1121,.T.);
#732=FACE_OUTER_BOUND('',#1122,.T.);
#733=FACE_OUTER_BOUND('',#1124,.T.);
#734=FACE_OUTER_BOUND('',#1126,.T.);
#735=FACE_OUTER_BOUND('',#1128,.T.);
#736=FACE_OUTER_BOUND('',#1130,.T.);
#737=EDGE_LOOP('',(#3646,#3647,#3648,#3649));
#738=EDGE_LOOP('',(#3650,#3651,#3652,#3653));
#739=EDGE_LOOP('',(#3654,#3655,#3656,#3657,#3658));
#740=EDGE_LOOP('',(#3659,#3660,#3661,#3662,#3663));
#741=EDGE_LOOP('',(#3664,#3665,#3666,#3667));
#742=EDGE_LOOP('',(#3668,#3669,#3670,#3671));
#743=EDGE_LOOP('',(#3672,#3673,#3674,#3675));
#744=EDGE_LOOP('',(#3676,#3677,#3678,#3679));
#745=EDGE_LOOP('',(#3680));
#746=EDGE_LOOP('',(#3681));
#747=EDGE_LOOP('',(#3682));
#748=EDGE_LOOP('',(#3683));
#749=EDGE_LOOP('',(#3684));
#750=EDGE_LOOP('',(#3685));
#751=EDGE_LOOP('',(#3686));
#752=EDGE_LOOP('',(#3687));
#753=EDGE_LOOP('',(#3688,#3689,#3690,#3691,#3692));
#754=EDGE_LOOP('',(#3693,#3694,#3695,#3696,#3697));
#755=EDGE_LOOP('',(#3698,#3699,#3700,#3701));
#756=EDGE_LOOP('',(#3702,#3703,#3704,#3705));
#757=EDGE_LOOP('',(#3706,#3707,#3708,#3709));
#758=EDGE_LOOP('',(#3710,#3711,#3712,#3713));
#759=EDGE_LOOP('',(#3714,#3715,#3716,#3717));
#760=EDGE_LOOP('',(#3718,#3719,#3720,#3721));
#761=EDGE_LOOP('',(#3722,#3723,#3724,#3725));
#762=EDGE_LOOP('',(#3726,#3727,#3728,#3729));
#763=EDGE_LOOP('',(#3730));
#764=EDGE_LOOP('',(#3731));
#765=EDGE_LOOP('',(#3732));
#766=EDGE_LOOP('',(#3733));
#767=EDGE_LOOP('',(#3734));
#768=EDGE_LOOP('',(#3735));
#769=EDGE_LOOP('',(#3736));
#770=EDGE_LOOP('',(#3737));
#771=EDGE_LOOP('',(#3738,#3739,#3740,#3741));
#772=EDGE_LOOP('',(#3742,#3743,#3744,#3745));
#773=EDGE_LOOP('',(#3746,#3747,#3748,#3749));
#774=EDGE_LOOP('',(#3750,#3751,#3752,#3753));
#775=EDGE_LOOP('',(#3754,#3755,#3756,#3757));
#776=EDGE_LOOP('',(#3758,#3759,#3760,#3761));
#777=EDGE_LOOP('',(#3762,#3763,#3764,#3765));
#778=EDGE_LOOP('',(#3766,#3767,#3768,#3769));
#779=EDGE_LOOP('',(#3770,#3771,#3772,#3773));
#780=EDGE_LOOP('',(#3774,#3775,#3776,#3777));
#781=EDGE_LOOP('',(#3778,#3779,#3780,#3781));
#782=EDGE_LOOP('',(#3782,#3783,#3784,#3785));
#783=EDGE_LOOP('',(#3786));
#784=EDGE_LOOP('',(#3787));
#785=EDGE_LOOP('',(#3788));
#786=EDGE_LOOP('',(#3789));
#787=EDGE_LOOP('',(#3790));
#788=EDGE_LOOP('',(#3791));
#789=EDGE_LOOP('',(#3792));
#790=EDGE_LOOP('',(#3793));
#791=EDGE_LOOP('',(#3794));
#792=EDGE_LOOP('',(#3795));
#793=EDGE_LOOP('',(#3796,#3797,#3798,#3799));
#794=EDGE_LOOP('',(#3800,#3801,#3802,#3803));
#795=EDGE_LOOP('',(#3804,#3805,#3806,#3807));
#796=EDGE_LOOP('',(#3808,#3809,#3810,#3811));
#797=EDGE_LOOP('',(#3812,#3813,#3814,#3815));
#798=EDGE_LOOP('',(#3816,#3817,#3818,#3819));
#799=EDGE_LOOP('',(#3820,#3821,#3822,#3823));
#800=EDGE_LOOP('',(#3824,#3825,#3826,#3827));
#801=EDGE_LOOP('',(#3828,#3829,#3830,#3831));
#802=EDGE_LOOP('',(#3832,#3833,#3834,#3835));
#803=EDGE_LOOP('',(#3836,#3837,#3838,#3839));
#804=EDGE_LOOP('',(#3840,#3841,#3842,#3843));
#805=EDGE_LOOP('',(#3844));
#806=EDGE_LOOP('',(#3845));
#807=EDGE_LOOP('',(#3846));
#808=EDGE_LOOP('',(#3847));
#809=EDGE_LOOP('',(#3848));
#810=EDGE_LOOP('',(#3849));
#811=EDGE_LOOP('',(#3850));
#812=EDGE_LOOP('',(#3851));
#813=EDGE_LOOP('',(#3852));
#814=EDGE_LOOP('',(#3853));
#815=EDGE_LOOP('',(#3854,#3855,#3856,#3857));
#816=EDGE_LOOP('',(#3858,#3859,#3860,#3861));
#817=EDGE_LOOP('',(#3862,#3863,#3864,#3865));
#818=EDGE_LOOP('',(#3866,#3867,#3868,#3869,#3870));
#819=EDGE_LOOP('',(#3871,#3872));
#820=EDGE_LOOP('',(#3873,#3874));
#821=EDGE_LOOP('',(#3875,#3876,#3877,#3878,#3879,#3880,#3881,#3882,#3883,
#3884,#3885,#3886));
#822=EDGE_LOOP('',(#3887,#3888,#3889,#3890));
#823=EDGE_LOOP('',(#3891));
#824=EDGE_LOOP('',(#3892));
#825=EDGE_LOOP('',(#3893));
#826=EDGE_LOOP('',(#3894,#3895,#3896,#3897));
#827=EDGE_LOOP('',(#3898,#3899,#3900,#3901));
#828=EDGE_LOOP('',(#3902,#3903,#3904,#3905));
#829=EDGE_LOOP('',(#3906,#3907,#3908,#3909));
#830=EDGE_LOOP('',(#3910,#3911,#3912,#3913));
#831=EDGE_LOOP('',(#3914,#3915,#3916,#3917));
#832=EDGE_LOOP('',(#3918,#3919,#3920,#3921));
#833=EDGE_LOOP('',(#3922));
#834=EDGE_LOOP('',(#3923));
#835=EDGE_LOOP('',(#3924,#3925,#3926,#3927));
#836=EDGE_LOOP('',(#3928));
#837=EDGE_LOOP('',(#3929));
#838=EDGE_LOOP('',(#3930,#3931,#3932,#3933));
#839=EDGE_LOOP('',(#3934,#3935,#3936,#3937));
#840=EDGE_LOOP('',(#3938));
#841=EDGE_LOOP('',(#3939));
#842=EDGE_LOOP('',(#3940));
#843=EDGE_LOOP('',(#3941));
#844=EDGE_LOOP('',(#3942,#3943,#3944,#3945));
#845=EDGE_LOOP('',(#3946,#3947,#3948,#3949));
#846=EDGE_LOOP('',(#3950,#3951,#3952,#3953));
#847=EDGE_LOOP('',(#3954,#3955,#3956,#3957));
#848=EDGE_LOOP('',(#3958,#3959,#3960,#3961));
#849=EDGE_LOOP('',(#3962));
#850=EDGE_LOOP('',(#3963));
#851=EDGE_LOOP('',(#3964));
#852=EDGE_LOOP('',(#3965));
#853=EDGE_LOOP('',(#3966,#3967,#3968,#3969));
#854=EDGE_LOOP('',(#3970,#3971,#3972,#3973));
#855=EDGE_LOOP('',(#3974));
#856=EDGE_LOOP('',(#3975));
#857=EDGE_LOOP('',(#3976));
#858=EDGE_LOOP('',(#3977));
#859=EDGE_LOOP('',(#3978,#3979,#3980,#3981,#3982));
#860=EDGE_LOOP('',(#3983,#3984,#3985,#3986,#3987,#3988));
#861=EDGE_LOOP('',(#3989));
#862=EDGE_LOOP('',(#3990,#3991,#3992,#3993,#3994));
#863=EDGE_LOOP('',(#3995,#3996,#3997,#3998,#3999,#4000,#4001));
#864=EDGE_LOOP('',(#4002));
#865=EDGE_LOOP('',(#4003));
#866=EDGE_LOOP('',(#4004,#4005,#4006,#4007,#4008,#4009,#4010,#4011,#4012));
#867=EDGE_LOOP('',(#4013,#4014));
#868=EDGE_LOOP('',(#4015));
#869=EDGE_LOOP('',(#4016,#4017,#4018,#4019));
#870=EDGE_LOOP('',(#4020,#4021,#4022,#4023));
#871=EDGE_LOOP('',(#4024,#4025,#4026,#4027));
#872=EDGE_LOOP('',(#4028,#4029,#4030,#4031));
#873=EDGE_LOOP('',(#4032,#4033,#4034,#4035));
#874=EDGE_LOOP('',(#4036,#4037,#4038,#4039));
#875=EDGE_LOOP('',(#4040,#4041,#4042,#4043));
#876=EDGE_LOOP('',(#4044,#4045,#4046,#4047));
#877=EDGE_LOOP('',(#4048,#4049,#4050,#4051));
#878=EDGE_LOOP('',(#4052,#4053,#4054,#4055));
#879=EDGE_LOOP('',(#4056,#4057,#4058,#4059));
#880=EDGE_LOOP('',(#4060,#4061,#4062,#4063));
#881=EDGE_LOOP('',(#4064,#4065,#4066,#4067));
#882=EDGE_LOOP('',(#4068,#4069,#4070,#4071));
#883=EDGE_LOOP('',(#4072,#4073,#4074,#4075));
#884=EDGE_LOOP('',(#4076,#4077,#4078,#4079));
#885=EDGE_LOOP('',(#4080,#4081,#4082,#4083));
#886=EDGE_LOOP('',(#4084,#4085,#4086,#4087));
#887=EDGE_LOOP('',(#4088,#4089,#4090,#4091));
#888=EDGE_LOOP('',(#4092,#4093,#4094,#4095));
#889=EDGE_LOOP('',(#4096,#4097,#4098,#4099));
#890=EDGE_LOOP('',(#4100,#4101,#4102,#4103));
#891=EDGE_LOOP('',(#4104,#4105,#4106,#4107));
#892=EDGE_LOOP('',(#4108,#4109,#4110,#4111));
#893=EDGE_LOOP('',(#4112,#4113,#4114,#4115));
#894=EDGE_LOOP('',(#4116,#4117,#4118,#4119));
#895=EDGE_LOOP('',(#4120,#4121,#4122,#4123));
#896=EDGE_LOOP('',(#4124,#4125,#4126,#4127));
#897=EDGE_LOOP('',(#4128,#4129,#4130,#4131));
#898=EDGE_LOOP('',(#4132,#4133,#4134,#4135));
#899=EDGE_LOOP('',(#4136,#4137,#4138,#4139));
#900=EDGE_LOOP('',(#4140,#4141,#4142,#4143));
#901=EDGE_LOOP('',(#4144,#4145,#4146,#4147));
#902=EDGE_LOOP('',(#4148,#4149,#4150,#4151));
#903=EDGE_LOOP('',(#4152,#4153,#4154,#4155));
#904=EDGE_LOOP('',(#4156,#4157,#4158,#4159));
#905=EDGE_LOOP('',(#4160,#4161,#4162,#4163));
#906=EDGE_LOOP('',(#4164,#4165,#4166,#4167));
#907=EDGE_LOOP('',(#4168,#4169,#4170,#4171));
#908=EDGE_LOOP('',(#4172,#4173,#4174,#4175));
#909=EDGE_LOOP('',(#4176,#4177,#4178,#4179));
#910=EDGE_LOOP('',(#4180,#4181,#4182,#4183));
#911=EDGE_LOOP('',(#4184,#4185,#4186,#4187));
#912=EDGE_LOOP('',(#4188,#4189,#4190,#4191));
#913=EDGE_LOOP('',(#4192,#4193,#4194,#4195));
#914=EDGE_LOOP('',(#4196,#4197,#4198,#4199));
#915=EDGE_LOOP('',(#4200,#4201,#4202,#4203));
#916=EDGE_LOOP('',(#4204,#4205,#4206,#4207));
#917=EDGE_LOOP('',(#4208,#4209,#4210,#4211));
#918=EDGE_LOOP('',(#4212,#4213,#4214,#4215));
#919=EDGE_LOOP('',(#4216,#4217,#4218,#4219));
#920=EDGE_LOOP('',(#4220,#4221,#4222,#4223));
#921=EDGE_LOOP('',(#4224,#4225,#4226,#4227));
#922=EDGE_LOOP('',(#4228,#4229,#4230,#4231));
#923=EDGE_LOOP('',(#4232,#4233,#4234,#4235));
#924=EDGE_LOOP('',(#4236,#4237,#4238,#4239));
#925=EDGE_LOOP('',(#4240,#4241,#4242,#4243));
#926=EDGE_LOOP('',(#4244,#4245,#4246,#4247));
#927=EDGE_LOOP('',(#4248,#4249,#4250,#4251));
#928=EDGE_LOOP('',(#4252,#4253,#4254,#4255));
#929=EDGE_LOOP('',(#4256,#4257,#4258,#4259));
#930=EDGE_LOOP('',(#4260,#4261,#4262,#4263));
#931=EDGE_LOOP('',(#4264,#4265,#4266,#4267));
#932=EDGE_LOOP('',(#4268,#4269,#4270,#4271));
#933=EDGE_LOOP('',(#4272,#4273,#4274,#4275));
#934=EDGE_LOOP('',(#4276,#4277,#4278,#4279));
#935=EDGE_LOOP('',(#4280,#4281,#4282,#4283));
#936=EDGE_LOOP('',(#4284,#4285,#4286,#4287));
#937=EDGE_LOOP('',(#4288,#4289,#4290,#4291));
#938=EDGE_LOOP('',(#4292,#4293,#4294,#4295));
#939=EDGE_LOOP('',(#4296,#4297,#4298,#4299));
#940=EDGE_LOOP('',(#4300,#4301,#4302,#4303));
#941=EDGE_LOOP('',(#4304,#4305,#4306,#4307));
#942=EDGE_LOOP('',(#4308,#4309,#4310,#4311));
#943=EDGE_LOOP('',(#4312,#4313,#4314,#4315));
#944=EDGE_LOOP('',(#4316,#4317,#4318,#4319));
#945=EDGE_LOOP('',(#4320,#4321,#4322,#4323));
#946=EDGE_LOOP('',(#4324,#4325,#4326,#4327));
#947=EDGE_LOOP('',(#4328,#4329,#4330,#4331));
#948=EDGE_LOOP('',(#4332,#4333,#4334,#4335));
#949=EDGE_LOOP('',(#4336,#4337,#4338,#4339));
#950=EDGE_LOOP('',(#4340,#4341,#4342,#4343));
#951=EDGE_LOOP('',(#4344,#4345,#4346,#4347));
#952=EDGE_LOOP('',(#4348,#4349,#4350,#4351));
#953=EDGE_LOOP('',(#4352,#4353,#4354,#4355));
#954=EDGE_LOOP('',(#4356,#4357,#4358,#4359));
#955=EDGE_LOOP('',(#4360,#4361,#4362,#4363));
#956=EDGE_LOOP('',(#4364,#4365,#4366,#4367));
#957=EDGE_LOOP('',(#4368,#4369,#4370,#4371));
#958=EDGE_LOOP('',(#4372,#4373,#4374,#4375));
#959=EDGE_LOOP('',(#4376,#4377,#4378,#4379));
#960=EDGE_LOOP('',(#4380,#4381,#4382,#4383));
#961=EDGE_LOOP('',(#4384,#4385,#4386,#4387));
#962=EDGE_LOOP('',(#4388,#4389,#4390,#4391));
#963=EDGE_LOOP('',(#4392,#4393,#4394,#4395));
#964=EDGE_LOOP('',(#4396,#4397,#4398,#4399));
#965=EDGE_LOOP('',(#4400,#4401,#4402,#4403));
#966=EDGE_LOOP('',(#4404,#4405,#4406,#4407));
#967=EDGE_LOOP('',(#4408,#4409,#4410,#4411));
#968=EDGE_LOOP('',(#4412,#4413,#4414,#4415));
#969=EDGE_LOOP('',(#4416,#4417,#4418,#4419));
#970=EDGE_LOOP('',(#4420,#4421,#4422,#4423));
#971=EDGE_LOOP('',(#4424,#4425,#4426,#4427));
#972=EDGE_LOOP('',(#4428,#4429,#4430,#4431));
#973=EDGE_LOOP('',(#4432,#4433,#4434,#4435));
#974=EDGE_LOOP('',(#4436,#4437,#4438,#4439));
#975=EDGE_LOOP('',(#4440,#4441,#4442,#4443));
#976=EDGE_LOOP('',(#4444,#4445,#4446,#4447));
#977=EDGE_LOOP('',(#4448,#4449,#4450,#4451));
#978=EDGE_LOOP('',(#4452,#4453,#4454,#4455));
#979=EDGE_LOOP('',(#4456,#4457,#4458,#4459));
#980=EDGE_LOOP('',(#4460,#4461,#4462,#4463));
#981=EDGE_LOOP('',(#4464,#4465,#4466,#4467));
#982=EDGE_LOOP('',(#4468,#4469,#4470,#4471));
#983=EDGE_LOOP('',(#4472,#4473,#4474,#4475));
#984=EDGE_LOOP('',(#4476,#4477,#4478,#4479));
#985=EDGE_LOOP('',(#4480,#4481,#4482,#4483));
#986=EDGE_LOOP('',(#4484,#4485,#4486,#4487));
#987=EDGE_LOOP('',(#4488,#4489,#4490,#4491));
#988=EDGE_LOOP('',(#4492,#4493,#4494,#4495));
#989=EDGE_LOOP('',(#4496,#4497,#4498,#4499));
#990=EDGE_LOOP('',(#4500,#4501,#4502,#4503));
#991=EDGE_LOOP('',(#4504,#4505,#4506,#4507));
#992=EDGE_LOOP('',(#4508,#4509,#4510,#4511));
#993=EDGE_LOOP('',(#4512,#4513,#4514,#4515));
#994=EDGE_LOOP('',(#4516,#4517,#4518,#4519));
#995=EDGE_LOOP('',(#4520,#4521,#4522,#4523));
#996=EDGE_LOOP('',(#4524,#4525,#4526,#4527));
#997=EDGE_LOOP('',(#4528,#4529,#4530,#4531));
#998=EDGE_LOOP('',(#4532,#4533,#4534,#4535));
#999=EDGE_LOOP('',(#4536,#4537,#4538,#4539));
#1000=EDGE_LOOP('',(#4540,#4541,#4542,#4543));
#1001=EDGE_LOOP('',(#4544,#4545,#4546,#4547));
#1002=EDGE_LOOP('',(#4548,#4549,#4550,#4551));
#1003=EDGE_LOOP('',(#4552,#4553,#4554,#4555));
#1004=EDGE_LOOP('',(#4556,#4557,#4558,#4559));
#1005=EDGE_LOOP('',(#4560,#4561,#4562,#4563));
#1006=EDGE_LOOP('',(#4564,#4565,#4566,#4567));
#1007=EDGE_LOOP('',(#4568,#4569,#4570,#4571));
#1008=EDGE_LOOP('',(#4572,#4573,#4574,#4575));
#1009=EDGE_LOOP('',(#4576,#4577,#4578,#4579));
#1010=EDGE_LOOP('',(#4580,#4581,#4582,#4583));
#1011=EDGE_LOOP('',(#4584,#4585,#4586,#4587));
#1012=EDGE_LOOP('',(#4588,#4589,#4590,#4591));
#1013=EDGE_LOOP('',(#4592,#4593,#4594,#4595));
#1014=EDGE_LOOP('',(#4596,#4597,#4598,#4599,#4600,#4601,#4602,#4603,#4604,
#4605,#4606,#4607,#4608,#4609,#4610,#4611,#4612,#4613,#4614,#4615,#4616,
#4617,#4618,#4619,#4620,#4621,#4622,#4623,#4624,#4625,#4626,#4627,#4628,
#4629,#4630,#4631,#4632,#4633,#4634,#4635,#4636,#4637,#4638,#4639,#4640,
#4641,#4642,#4643,#4644,#4645,#4646,#4647,#4648,#4649,#4650,#4651,#4652,
#4653,#4654,#4655,#4656,#4657,#4658,#4659,#4660,#4661,#4662,#4663,#4664,
#4665,#4666,#4667,#4668,#4669,#4670,#4671,#4672,#4673,#4674,#4675,#4676,
#4677,#4678,#4679,#4680,#4681,#4682,#4683,#4684,#4685,#4686,#4687,#4688,
#4689,#4690,#4691,#4692,#4693,#4694,#4695,#4696,#4697,#4698,#4699,#4700,
#4701,#4702,#4703,#4704,#4705,#4706,#4707,#4708,#4709,#4710,#4711,#4712,
#4713,#4714,#4715));
#1015=EDGE_LOOP('',(#4716,#4717,#4718,#4719));
#1016=EDGE_LOOP('',(#4720,#4721,#4722,#4723));
#1017=EDGE_LOOP('',(#4724,#4725,#4726,#4727));
#1018=EDGE_LOOP('',(#4728,#4729,#4730,#4731));
#1019=EDGE_LOOP('',(#4732,#4733,#4734,#4735));
#1020=EDGE_LOOP('',(#4736));
#1021=EDGE_LOOP('',(#4737,#4738,#4739,#4740));
#1022=EDGE_LOOP('',(#4741,#4742,#4743,#4744,#4745,#4746,#4747,#4748,#4749,
#4750,#4751,#4752,#4753,#4754,#4755,#4756,#4757,#4758,#4759,#4760,#4761,
#4762,#4763,#4764,#4765,#4766,#4767,#4768,#4769,#4770,#4771,#4772,#4773,
#4774,#4775,#4776,#4777,#4778,#4779,#4780,#4781,#4782,#4783,#4784,#4785,
#4786,#4787,#4788,#4789,#4790,#4791,#4792,#4793,#4794,#4795,#4796,#4797,
#4798,#4799,#4800,#4801,#4802,#4803,#4804,#4805,#4806,#4807,#4808,#4809,
#4810,#4811,#4812,#4813,#4814,#4815,#4816,#4817,#4818,#4819,#4820,#4821,
#4822,#4823,#4824,#4825,#4826,#4827,#4828,#4829,#4830,#4831,#4832,#4833,
#4834,#4835,#4836,#4837,#4838,#4839,#4840,#4841,#4842,#4843,#4844,#4845,
#4846,#4847,#4848,#4849,#4850,#4851,#4852,#4853,#4854,#4855,#4856,#4857,
#4858,#4859,#4860));
#1023=EDGE_LOOP('',(#4861,#4862,#4863,#4864));
#1024=EDGE_LOOP('',(#4865,#4866,#4867,#4868));
#1025=EDGE_LOOP('',(#4869,#4870,#4871,#4872));
#1026=EDGE_LOOP('',(#4873,#4874,#4875,#4876));
#1027=EDGE_LOOP('',(#4877,#4878,#4879,#4880));
#1028=EDGE_LOOP('',(#4881));
#1029=EDGE_LOOP('',(#4882,#4883,#4884,#4885));
#1030=EDGE_LOOP('',(#4886,#4887,#4888,#4889));
#1031=EDGE_LOOP('',(#4890));
#1032=EDGE_LOOP('',(#4891));
#1033=EDGE_LOOP('',(#4892,#4893,#4894,#4895,#4896,#4897,#4898,#4899,#4900,
#4901,#4902,#4903,#4904,#4905,#4906,#4907));
#1034=EDGE_LOOP('',(#4908));
#1035=EDGE_LOOP('',(#4909,#4910,#4911,#4912));
#1036=EDGE_LOOP('',(#4913,#4914,#4915,#4916));
#1037=EDGE_LOOP('',(#4917,#4918,#4919,#4920));
#1038=EDGE_LOOP('',(#4921,#4922,#4923,#4924));
#1039=EDGE_LOOP('',(#4925,#4926,#4927,#4928));
#1040=EDGE_LOOP('',(#4929,#4930,#4931,#4932));
#1041=EDGE_LOOP('',(#4933,#4934,#4935,#4936,#4937,#4938,#4939,#4940,#4941,
#4942,#4943,#4944,#4945,#4946,#4947,#4948));
#1042=EDGE_LOOP('',(#4949));
#1043=EDGE_LOOP('',(#4950,#4951,#4952,#4953));
#1044=EDGE_LOOP('',(#4954,#4955,#4956,#4957));
#1045=EDGE_LOOP('',(#4958,#4959,#4960,#4961));
#1046=EDGE_LOOP('',(#4962,#4963,#4964,#4965));
#1047=EDGE_LOOP('',(#4966,#4967,#4968,#4969));
#1048=EDGE_LOOP('',(#4970,#4971,#4972,#4973));
#1049=EDGE_LOOP('',(#4974,#4975,#4976,#4977));
#1050=EDGE_LOOP('',(#4978,#4979,#4980,#4981));
#1051=EDGE_LOOP('',(#4982,#4983,#4984,#4985));
#1052=EDGE_LOOP('',(#4986,#4987,#4988,#4989));
#1053=EDGE_LOOP('',(#4990,#4991,#4992,#4993));
#1054=EDGE_LOOP('',(#4994,#4995,#4996,#4997));
#1055=EDGE_LOOP('',(#4998,#4999,#5000,#5001));
#1056=EDGE_LOOP('',(#5002,#5003,#5004,#5005,#5006));
#1057=EDGE_LOOP('',(#5007,#5008,#5009,#5010,#5011));
#1058=EDGE_LOOP('',(#5012,#5013,#5014,#5015));
#1059=EDGE_LOOP('',(#5016,#5017,#5018,#5019));
#1060=EDGE_LOOP('',(#5020,#5021,#5022,#5023));
#1061=EDGE_LOOP('',(#5024,#5025,#5026,#5027));
#1062=EDGE_LOOP('',(#5028));
#1063=EDGE_LOOP('',(#5029));
#1064=EDGE_LOOP('',(#5030));
#1065=EDGE_LOOP('',(#5031));
#1066=EDGE_LOOP('',(#5032));
#1067=EDGE_LOOP('',(#5033));
#1068=EDGE_LOOP('',(#5034));
#1069=EDGE_LOOP('',(#5035));
#1070=EDGE_LOOP('',(#5036,#5037,#5038,#5039,#5040));
#1071=EDGE_LOOP('',(#5041,#5042,#5043,#5044,#5045));
#1072=EDGE_LOOP('',(#5046,#5047,#5048,#5049));
#1073=EDGE_LOOP('',(#5050,#5051,#5052,#5053));
#1074=EDGE_LOOP('',(#5054,#5055,#5056,#5057));
#1075=EDGE_LOOP('',(#5058,#5059,#5060,#5061));
#1076=EDGE_LOOP('',(#5062,#5063,#5064,#5065));
#1077=EDGE_LOOP('',(#5066,#5067,#5068,#5069));
#1078=EDGE_LOOP('',(#5070,#5071,#5072,#5073));
#1079=EDGE_LOOP('',(#5074,#5075,#5076,#5077));
#1080=EDGE_LOOP('',(#5078));
#1081=EDGE_LOOP('',(#5079));
#1082=EDGE_LOOP('',(#5080));
#1083=EDGE_LOOP('',(#5081));
#1084=EDGE_LOOP('',(#5082));
#1085=EDGE_LOOP('',(#5083));
#1086=EDGE_LOOP('',(#5084));
#1087=EDGE_LOOP('',(#5085));
#1088=EDGE_LOOP('',(#5086,#5087,#5088,#5089));
#1089=EDGE_LOOP('',(#5090,#5091,#5092,#5093));
#1090=EDGE_LOOP('',(#5094,#5095,#5096,#5097));
#1091=EDGE_LOOP('',(#5098,#5099,#5100,#5101));
#1092=EDGE_LOOP('',(#5102,#5103,#5104,#5105));
#1093=EDGE_LOOP('',(#5106,#5107,#5108,#5109));
#1094=EDGE_LOOP('',(#5110,#5111,#5112,#5113));
#1095=EDGE_LOOP('',(#5114,#5115,#5116,#5117));
#1096=EDGE_LOOP('',(#5118,#5119,#5120,#5121));
#1097=EDGE_LOOP('',(#5122,#5123,#5124,#5125));
#1098=EDGE_LOOP('',(#5126,#5127,#5128,#5129));
#1099=EDGE_LOOP('',(#5130,#5131,#5132,#5133));
#1100=EDGE_LOOP('',(#5134));
#1101=EDGE_LOOP('',(#5135));
#1102=EDGE_LOOP('',(#5136));
#1103=EDGE_LOOP('',(#5137));
#1104=EDGE_LOOP('',(#5138));
#1105=EDGE_LOOP('',(#5139));
#1106=EDGE_LOOP('',(#5140));
#1107=EDGE_LOOP('',(#5141));
#1108=EDGE_LOOP('',(#5142));
#1109=EDGE_LOOP('',(#5143));
#1110=EDGE_LOOP('',(#5144,#5145,#5146,#5147));
#1111=EDGE_LOOP('',(#5148,#5149,#5150,#5151));
#1112=EDGE_LOOP('',(#5152,#5153,#5154,#5155));
#1113=EDGE_LOOP('',(#5156,#5157,#5158,#5159));
#1114=EDGE_LOOP('',(#5160,#5161,#5162,#5163));
#1115=EDGE_LOOP('',(#5164,#5165,#5166,#5167));
#1116=EDGE_LOOP('',(#5168,#5169,#5170,#5171));
#1117=EDGE_LOOP('',(#5172,#5173,#5174,#5175));
#1118=EDGE_LOOP('',(#5176,#5177,#5178,#5179));
#1119=EDGE_LOOP('',(#5180,#5181,#5182,#5183));
#1120=EDGE_LOOP('',(#5184,#5185,#5186,#5187));
#1121=EDGE_LOOP('',(#5188,#5189,#5190,#5191));
#1122=EDGE_LOOP('',(#5192));
#1123=EDGE_LOOP('',(#5193));
#1124=EDGE_LOOP('',(#5194));
#1125=EDGE_LOOP('',(#5195));
#1126=EDGE_LOOP('',(#5196));
#1127=EDGE_LOOP('',(#5197));
#1128=EDGE_LOOP('',(#5198));
#1129=EDGE_LOOP('',(#5199));
#1130=EDGE_LOOP('',(#5200));
#1131=EDGE_LOOP('',(#5201));
#1132=LINE('',#8145,#1596);
#1133=LINE('',#8151,#1597);
#1134=LINE('',#8159,#1598);
#1135=LINE('',#8163,#1599);
#1136=LINE('',#8174,#1600);
#1137=LINE('',#8181,#1601);
#1138=LINE('',#8192,#1602);
#1139=LINE('',#8197,#1603);
#1140=LINE('',#8207,#1604);
#1141=LINE('',#8217,#1605);
#1142=LINE('',#8221,#1606);
#1143=LINE('',#8231,#1607);
#1144=LINE('',#8245,#1608);
#1145=LINE('',#8256,#1609);
#1146=LINE('',#8270,#1610);
#1147=LINE('',#8284,#1611);
#1148=LINE('',#8298,#1612);
#1149=LINE('',#8308,#1613);
#1150=LINE('',#8319,#1614);
#1151=LINE('',#8333,#1615);
#1152=LINE('',#8347,#1616);
#1153=LINE('',#8361,#1617);
#1154=LINE('',#8372,#1618);
#1155=LINE('',#8388,#1619);
#1156=LINE('',#8400,#1620);
#1157=LINE('',#8415,#1621);
#1158=LINE('',#8427,#1622);
#1159=LINE('',#8444,#1623);
#1160=LINE('',#8452,#1624);
#1161=LINE('',#8456,#1625);
#1162=LINE('',#8458,#1626);
#1163=LINE('',#8464,#1627);
#1164=LINE('',#8470,#1628);
#1165=LINE('',#8476,#1629);
#1166=LINE('',#8482,#1630);
#1167=LINE('',#8488,#1631);
#1168=LINE('',#8490,#1632);
#1169=LINE('',#8492,#1633);
#1170=LINE('',#8493,#1634);
#1171=LINE('',#8500,#1635);
#1172=LINE('',#8505,#1636);
#1173=LINE('',#8510,#1637);
#1174=LINE('',#8512,#1638);
#1175=LINE('',#8513,#1639);
#1176=LINE('',#8516,#1640);
#1177=LINE('',#8517,#1641);
#1178=LINE('',#8520,#1642);
#1179=LINE('',#8521,#1643);
#1180=LINE('',#8523,#1644);
#1181=LINE('',#8531,#1645);
#1182=LINE('',#8537,#1646);
#1183=LINE('',#8552,#1647);
#1184=LINE('',#8641,#1648);
#1185=LINE('',#8649,#1649);
#1186=LINE('',#8650,#1650);
#1187=LINE('',#8656,#1651);
#1188=LINE('',#8658,#1652);
#1189=LINE('',#8660,#1653);
#1190=LINE('',#8661,#1654);
#1191=LINE('',#8664,#1655);
#1192=LINE('',#8666,#1656);
#1193=LINE('',#8667,#1657);
#1194=LINE('',#8670,#1658);
#1195=LINE('',#8672,#1659);
#1196=LINE('',#8673,#1660);
#1197=LINE('',#8678,#1661);
#1198=LINE('',#8684,#1662);
#1199=LINE('',#8689,#1663);
#1200=LINE('',#8691,#1664);
#1201=LINE('',#8693,#1665);
#1202=LINE('',#8694,#1666);
#1203=LINE('',#8697,#1667);
#1204=LINE('',#8699,#1668);
#1205=LINE('',#8700,#1669);
#1206=LINE('',#8702,#1670);
#1207=LINE('',#8703,#1671);
#1208=LINE('',#8708,#1672);
#1209=LINE('',#8713,#1673);
#1210=LINE('',#8715,#1674);
#1211=LINE('',#8717,#1675);
#1212=LINE('',#8718,#1676);
#1213=LINE('',#8721,#1677);
#1214=LINE('',#8723,#1678);
#1215=LINE('',#8724,#1679);
#1216=LINE('',#8726,#1680);
#1217=LINE('',#8727,#1681);
#1218=LINE('',#8732,#1682);
#1219=LINE('',#8737,#1683);
#1220=LINE('',#8739,#1684);
#1221=LINE('',#8741,#1685);
#1222=LINE('',#8742,#1686);
#1223=LINE('',#8745,#1687);
#1224=LINE('',#8747,#1688);
#1225=LINE('',#8748,#1689);
#1226=LINE('',#8750,#1690);
#1227=LINE('',#8751,#1691);
#1228=LINE('',#8756,#1692);
#1229=LINE('',#8761,#1693);
#1230=LINE('',#8763,#1694);
#1231=LINE('',#8765,#1695);
#1232=LINE('',#8766,#1696);
#1233=LINE('',#8769,#1697);
#1234=LINE('',#8771,#1698);
#1235=LINE('',#8772,#1699);
#1236=LINE('',#8774,#1700);
#1237=LINE('',#8775,#1701);
#1238=LINE('',#8780,#1702);
#1239=LINE('',#8785,#1703);
#1240=LINE('',#8787,#1704);
#1241=LINE('',#8789,#1705);
#1242=LINE('',#8790,#1706);
#1243=LINE('',#8793,#1707);
#1244=LINE('',#8795,#1708);
#1245=LINE('',#8796,#1709);
#1246=LINE('',#8799,#1710);
#1247=LINE('',#8801,#1711);
#1248=LINE('',#8802,#1712);
#1249=LINE('',#8807,#1713);
#1250=LINE('',#8813,#1714);
#1251=LINE('',#8818,#1715);
#1252=LINE('',#8820,#1716);
#1253=LINE('',#8822,#1717);
#1254=LINE('',#8823,#1718);
#1255=LINE('',#8825,#1719);
#1256=LINE('',#8826,#1720);
#1257=LINE('',#8828,#1721);
#1258=LINE('',#8829,#1722);
#1259=LINE('',#8833,#1723);
#1260=LINE('',#8835,#1724);
#1261=LINE('',#8837,#1725);
#1262=LINE('',#8838,#1726);
#1263=LINE('',#8841,#1727);
#1264=LINE('',#8843,#1728);
#1265=LINE('',#8844,#1729);
#1266=LINE('',#8846,#1730);
#1267=LINE('',#8847,#1731);
#1268=LINE('',#8852,#1732);
#1269=LINE('',#8857,#1733);
#1270=LINE('',#8859,#1734);
#1271=LINE('',#8861,#1735);
#1272=LINE('',#8862,#1736);
#1273=LINE('',#8865,#1737);
#1274=LINE('',#8867,#1738);
#1275=LINE('',#8868,#1739);
#1276=LINE('',#8871,#1740);
#1277=LINE('',#8873,#1741);
#1278=LINE('',#8874,#1742);
#1279=LINE('',#8879,#1743);
#1280=LINE('',#8885,#1744);
#1281=LINE('',#8890,#1745);
#1282=LINE('',#8892,#1746);
#1283=LINE('',#8894,#1747);
#1284=LINE('',#8895,#1748);
#1285=LINE('',#8898,#1749);
#1286=LINE('',#8900,#1750);
#1287=LINE('',#8901,#1751);
#1288=LINE('',#8904,#1752);
#1289=LINE('',#8906,#1753);
#1290=LINE('',#8907,#1754);
#1291=LINE('',#8912,#1755);
#1292=LINE('',#8918,#1756);
#1293=LINE('',#8923,#1757);
#1294=LINE('',#8925,#1758);
#1295=LINE('',#8927,#1759);
#1296=LINE('',#8928,#1760);
#1297=LINE('',#8930,#1761);
#1298=LINE('',#8931,#1762);
#1299=LINE('',#8933,#1763);
#1300=LINE('',#8934,#1764);
#1301=LINE('',#8938,#1765);
#1302=LINE('',#8940,#1766);
#1303=LINE('',#8942,#1767);
#1304=LINE('',#8943,#1768);
#1305=LINE('',#8945,#1769);
#1306=LINE('',#8946,#1770);
#1307=LINE('',#8948,#1771);
#1308=LINE('',#8949,#1772);
#1309=LINE('',#8953,#1773);
#1310=LINE('',#8955,#1774);
#1311=LINE('',#8957,#1775);
#1312=LINE('',#8958,#1776);
#1313=LINE('',#8961,#1777);
#1314=LINE('',#8963,#1778);
#1315=LINE('',#8964,#1779);
#1316=LINE('',#8966,#1780);
#1317=LINE('',#8967,#1781);
#1318=LINE('',#8972,#1782);
#1319=LINE('',#8977,#1783);
#1320=LINE('',#8979,#1784);
#1321=LINE('',#8981,#1785);
#1322=LINE('',#8982,#1786);
#1323=LINE('',#8985,#1787);
#1324=LINE('',#8987,#1788);
#1325=LINE('',#8988,#1789);
#1326=LINE('',#8990,#1790);
#1327=LINE('',#8991,#1791);
#1328=LINE('',#8996,#1792);
#1329=LINE('',#9001,#1793);
#1330=LINE('',#9003,#1794);
#1331=LINE('',#9005,#1795);
#1332=LINE('',#9006,#1796);
#1333=LINE('',#9009,#1797);
#1334=LINE('',#9011,#1798);
#1335=LINE('',#9012,#1799);
#1336=LINE('',#9015,#1800);
#1337=LINE('',#9017,#1801);
#1338=LINE('',#9018,#1802);
#1339=LINE('',#9023,#1803);
#1340=LINE('',#9029,#1804);
#1341=LINE('',#9034,#1805);
#1342=LINE('',#9036,#1806);
#1343=LINE('',#9038,#1807);
#1344=LINE('',#9039,#1808);
#1345=LINE('',#9042,#1809);
#1346=LINE('',#9044,#1810);
#1347=LINE('',#9045,#1811);
#1348=LINE('',#9047,#1812);
#1349=LINE('',#9048,#1813);
#1350=LINE('',#9053,#1814);
#1351=LINE('',#9058,#1815);
#1352=LINE('',#9060,#1816);
#1353=LINE('',#9062,#1817);
#1354=LINE('',#9063,#1818);
#1355=LINE('',#9066,#1819);
#1356=LINE('',#9068,#1820);
#1357=LINE('',#9069,#1821);
#1358=LINE('',#9071,#1822);
#1359=LINE('',#9072,#1823);
#1360=LINE('',#9077,#1824);
#1361=LINE('',#9082,#1825);
#1362=LINE('',#9084,#1826);
#1363=LINE('',#9086,#1827);
#1364=LINE('',#9087,#1828);
#1365=LINE('',#9089,#1829);
#1366=LINE('',#9090,#1830);
#1367=LINE('',#9092,#1831);
#1368=LINE('',#9093,#1832);
#1369=LINE('',#9097,#1833);
#1370=LINE('',#9099,#1834);
#1371=LINE('',#9101,#1835);
#1372=LINE('',#9102,#1836);
#1373=LINE('',#9105,#1837);
#1374=LINE('',#9107,#1838);
#1375=LINE('',#9108,#1839);
#1376=LINE('',#9111,#1840);
#1377=LINE('',#9113,#1841);
#1378=LINE('',#9114,#1842);
#1379=LINE('',#9119,#1843);
#1380=LINE('',#9125,#1844);
#1381=LINE('',#9130,#1845);
#1382=LINE('',#9132,#1846);
#1383=LINE('',#9134,#1847);
#1384=LINE('',#9135,#1848);
#1385=LINE('',#9137,#1849);
#1386=LINE('',#9138,#1850);
#1387=LINE('',#9140,#1851);
#1388=LINE('',#9141,#1852);
#1389=LINE('',#9145,#1853);
#1390=LINE('',#9147,#1854);
#1391=LINE('',#9149,#1855);
#1392=LINE('',#9150,#1856);
#1393=LINE('',#9153,#1857);
#1394=LINE('',#9155,#1858);
#1395=LINE('',#9156,#1859);
#1396=LINE('',#9159,#1860);
#1397=LINE('',#9161,#1861);
#1398=LINE('',#9162,#1862);
#1399=LINE('',#9167,#1863);
#1400=LINE('',#9173,#1864);
#1401=LINE('',#9178,#1865);
#1402=LINE('',#9180,#1866);
#1403=LINE('',#9182,#1867);
#1404=LINE('',#9183,#1868);
#1405=LINE('',#9185,#1869);
#1406=LINE('',#9186,#1870);
#1407=LINE('',#9188,#1871);
#1408=LINE('',#9189,#1872);
#1409=LINE('',#9193,#1873);
#1410=LINE('',#9195,#1874);
#1411=LINE('',#9197,#1875);
#1412=LINE('',#9198,#1876);
#1413=LINE('',#9201,#1877);
#1414=LINE('',#9203,#1878);
#1415=LINE('',#9204,#1879);
#1416=LINE('',#9207,#1880);
#1417=LINE('',#9209,#1881);
#1418=LINE('',#9210,#1882);
#1419=LINE('',#9215,#1883);
#1420=LINE('',#9221,#1884);
#1421=LINE('',#9226,#1885);
#1422=LINE('',#9228,#1886);
#1423=LINE('',#9230,#1887);
#1424=LINE('',#9231,#1888);
#1425=LINE('',#9234,#1889);
#1426=LINE('',#9236,#1890);
#1427=LINE('',#9237,#1891);
#1428=LINE('',#9239,#1892);
#1429=LINE('',#9240,#1893);
#1430=LINE('',#9245,#1894);
#1431=LINE('',#9250,#1895);
#1432=LINE('',#9252,#1896);
#1433=LINE('',#9254,#1897);
#1434=LINE('',#9255,#1898);
#1435=LINE('',#9258,#1899);
#1436=LINE('',#9260,#1900);
#1437=LINE('',#9261,#1901);
#1438=LINE('',#9263,#1902);
#1439=LINE('',#9264,#1903);
#1440=LINE('',#9269,#1904);
#1441=LINE('',#9274,#1905);
#1442=LINE('',#9276,#1906);
#1443=LINE('',#9278,#1907);
#1444=LINE('',#9279,#1908);
#1445=LINE('',#9281,#1909);
#1446=LINE('',#9282,#1910);
#1447=LINE('',#9285,#1911);
#1448=LINE('',#9287,#1912);
#1449=LINE('',#9288,#1913);
#1450=LINE('',#9293,#1914);
#1451=LINE('',#9298,#1915);
#1452=LINE('',#9300,#1916);
#1453=LINE('',#9302,#1917);
#1454=LINE('',#9303,#1918);
#1455=LINE('',#9306,#1919);
#1456=LINE('',#9308,#1920);
#1457=LINE('',#9309,#1921);
#1458=LINE('',#9312,#1922);
#1459=LINE('',#9314,#1923);
#1460=LINE('',#9315,#1924);
#1461=LINE('',#9320,#1925);
#1462=LINE('',#9326,#1926);
#1463=LINE('',#9331,#1927);
#1464=LINE('',#9333,#1928);
#1465=LINE('',#9335,#1929);
#1466=LINE('',#9336,#1930);
#1467=LINE('',#9338,#1931);
#1468=LINE('',#9339,#1932);
#1469=LINE('',#9341,#1933);
#1470=LINE('',#9342,#1934);
#1471=LINE('',#9346,#1935);
#1472=LINE('',#9348,#1936);
#1473=LINE('',#9350,#1937);
#1474=LINE('',#9351,#1938);
#1475=LINE('',#9353,#1939);
#1476=LINE('',#9354,#1940);
#1477=LINE('',#9356,#1941);
#1478=LINE('',#9357,#1942);
#1479=LINE('',#9361,#1943);
#1480=LINE('',#9363,#1944);
#1481=LINE('',#9365,#1945);
#1482=LINE('',#9366,#1946);
#1483=LINE('',#9368,#1947);
#1484=LINE('',#9369,#1948);
#1485=LINE('',#9371,#1949);
#1486=LINE('',#9372,#1950);
#1487=LINE('',#9376,#1951);
#1488=LINE('',#9378,#1952);
#1489=LINE('',#9380,#1953);
#1490=LINE('',#9381,#1954);
#1491=LINE('',#9385,#1955);
#1492=LINE('',#9387,#1956);
#1493=LINE('',#9389,#1957);
#1494=LINE('',#9390,#1958);
#1495=LINE('',#9395,#1959);
#1496=LINE('',#9401,#1960);
#1497=LINE('',#9407,#1961);
#1498=LINE('',#9413,#1962);
#1499=LINE('',#9416,#1963);
#1500=LINE('',#9417,#1964);
#1501=LINE('',#9421,#1965);
#1502=LINE('',#9423,#1966);
#1503=LINE('',#9425,#1967);
#1504=LINE('',#9426,#1968);
#1505=LINE('',#9431,#1969);
#1506=LINE('',#9437,#1970);
#1507=LINE('',#9440,#1971);
#1508=LINE('',#9441,#1972);
#1509=LINE('',#9445,#1973);
#1510=LINE('',#9447,#1974);
#1511=LINE('',#9449,#1975);
#1512=LINE('',#9450,#1976);
#1513=LINE('',#9455,#1977);
#1514=LINE('',#9461,#1978);
#1515=LINE('',#9464,#1979);
#1516=LINE('',#9465,#1980);
#1517=LINE('',#9469,#1981);
#1518=LINE('',#9471,#1982);
#1519=LINE('',#9473,#1983);
#1520=LINE('',#9474,#1984);
#1521=LINE('',#9479,#1985);
#1522=LINE('',#9485,#1986);
#1523=LINE('',#9488,#1987);
#1524=LINE('',#9489,#1988);
#1525=LINE('',#9493,#1989);
#1526=LINE('',#9495,#1990);
#1527=LINE('',#9497,#1991);
#1528=LINE('',#9498,#1992);
#1529=LINE('',#9503,#1993);
#1530=LINE('',#9509,#1994);
#1531=LINE('',#9512,#1995);
#1532=LINE('',#9513,#1996);
#1533=LINE('',#9515,#1997);
#1534=LINE('',#9516,#1998);
#1535=LINE('',#9521,#1999);
#1536=LINE('',#9530,#2000);
#1537=LINE('',#9538,#2001);
#1538=LINE('',#9540,#2002);
#1539=LINE('',#9542,#2003);
#1540=LINE('',#9546,#2004);
#1541=LINE('',#9550,#2005);
#1542=LINE('',#9554,#2006);
#1543=LINE('',#9558,#2007);
#1544=LINE('',#9560,#2008);
#1545=LINE('',#9562,#2009);
#1546=LINE('',#9566,#2010);
#1547=LINE('',#9570,#2011);
#1548=LINE('',#9572,#2012);
#1549=LINE('',#9573,#2013);
#1550=LINE('',#9578,#2014);
#1551=LINE('',#9579,#2015);
#1552=LINE('',#9582,#2016);
#1553=LINE('',#9583,#2017);
#1554=LINE('',#9587,#2018);
#1555=LINE('',#9590,#2019);
#1556=LINE('',#9591,#2020);
#1557=LINE('',#9593,#2021);
#1558=LINE('',#9596,#2022);
#1559=LINE('',#9598,#2023);
#1560=LINE('',#9602,#2024);
#1561=LINE('',#9606,#2025);
#1562=LINE('',#9610,#2026);
#1563=LINE('',#9613,#2027);
#1564=LINE('',#9617,#2028);
#1565=LINE('',#9619,#2029);
#1566=LINE('',#9621,#2030);
#1567=LINE('',#9623,#2031);
#1568=LINE('',#9625,#2032);
#1569=LINE('',#9627,#2033);
#1570=LINE('',#9629,#2034);
#1571=LINE('',#9631,#2035);
#1572=LINE('',#9633,#2036);
#1573=LINE('',#9635,#2037);
#1574=LINE('',#9642,#2038);
#1575=LINE('',#9648,#2039);
#1576=LINE('',#9656,#2040);
#1577=LINE('',#9660,#2041);
#1578=LINE('',#9671,#2042);
#1579=LINE('',#9678,#2043);
#1580=LINE('',#9689,#2044);
#1581=LINE('',#9694,#2045);
#1582=LINE('',#9704,#2046);
#1583=LINE('',#9714,#2047);
#1584=LINE('',#9718,#2048);
#1585=LINE('',#9728,#2049);
#1586=LINE('',#9742,#2050);
#1587=LINE('',#9753,#2051);
#1588=LINE('',#9767,#2052);
#1589=LINE('',#9781,#2053);
#1590=LINE('',#9795,#2054);
#1591=LINE('',#9805,#2055);
#1592=LINE('',#9816,#2056);
#1593=LINE('',#9830,#2057);
#1594=LINE('',#9844,#2058);
#1595=LINE('',#9858,#2059);
#1596=VECTOR('',#6379,4.8);
#1597=VECTOR('',#6386,4.872);
#1598=VECTOR('',#6395,4.8);
#1599=VECTOR('',#6400,4.8);
#1600=VECTOR('',#6415,6.);
#1601=VECTOR('',#6424,4.845);
#1602=VECTOR('',#6439,3.1184375);
#1603=VECTOR('',#6446,3.1184375);
#1604=VECTOR('',#6459,3.272);
#1605=VECTOR('',#6472,3.1184375);
#1606=VECTOR('',#6477,3.0734375);
#1607=VECTOR('',#6490,2.);
#1608=VECTOR('',#6511,3.2);
#1609=VECTOR('',#6526,4.36638040039984);
#1610=VECTOR('',#6545,4.57071796769724);
#1611=VECTOR('',#6564,4.62071796769724);
#1612=VECTOR('',#6583,4.27977786002139);
#1613=VECTOR('',#6598,3.2);
#1614=VECTOR('',#6613,4.36638040039984);
#1615=VECTOR('',#6632,4.57071796769724);
#1616=VECTOR('',#6651,4.62071796769724);
#1617=VECTOR('',#6670,4.27977786002139);
#1618=VECTOR('',#6687,1.8052925);
#1619=VECTOR('',#6692,10.);
#1620=VECTOR('',#6693,10.);
#1621=VECTOR('',#6696,10.);
#1622=VECTOR('',#6697,10.);
#1623=VECTOR('',#6724,3.8950136037689);
#1624=VECTOR('',#6735,1.78525000000062);
#1625=VECTOR('',#6740,1.89262500000135);
#1626=VECTOR('',#6743,1.954);
#1627=VECTOR('',#6750,2.);
#1628=VECTOR('',#6757,2.);
#1629=VECTOR('',#6764,6.00000000000001);
#1630=VECTOR('',#6771,7.00000000000001);
#1631=VECTOR('',#6778,10.);
#1632=VECTOR('',#6779,10.);
#1633=VECTOR('',#6780,10.);
#1634=VECTOR('',#6781,10.);
#1635=VECTOR('',#6788,6.00000000000001);
#1636=VECTOR('',#6795,7.00000000000001);
#1637=VECTOR('',#6802,10.);
#1638=VECTOR('',#6803,10.);
#1639=VECTOR('',#6804,10.);
#1640=VECTOR('',#6807,10.);
#1641=VECTOR('',#6808,10.);
#1642=VECTOR('',#6811,10.);
#1643=VECTOR('',#6812,10.);
#1644=VECTOR('',#6815,10.);
#1645=VECTOR('',#6826,1.99999999999999);
#1646=VECTOR('',#6833,2.99999999999999);
#1647=VECTOR('',#6854,0.770000000000005);
#1648=VECTOR('',#6869,0.770000000000005);
#1649=VECTOR('',#6880,1.99999999999999);
#1650=VECTOR('',#6881,1.99999999999999);
#1651=VECTOR('',#6888,10.);
#1652=VECTOR('',#6889,10.);
#1653=VECTOR('',#6890,10.);
#1654=VECTOR('',#6891,10.);
#1655=VECTOR('',#6894,10.);
#1656=VECTOR('',#6895,10.);
#1657=VECTOR('',#6896,10.);
#1658=VECTOR('',#6899,10.);
#1659=VECTOR('',#6900,10.);
#1660=VECTOR('',#6901,10.);
#1661=VECTOR('',#6906,10.);
#1662=VECTOR('',#6913,10.);
#1663=VECTOR('',#6918,10.);
#1664=VECTOR('',#6919,10.);
#1665=VECTOR('',#6920,10.);
#1666=VECTOR('',#6921,10.);
#1667=VECTOR('',#6924,10.);
#1668=VECTOR('',#6925,10.);
#1669=VECTOR('',#6926,10.);
#1670=VECTOR('',#6929,10.);
#1671=VECTOR('',#6930,10.);
#1672=VECTOR('',#6935,10.);
#1673=VECTOR('',#6940,10.);
#1674=VECTOR('',#6941,10.);
#1675=VECTOR('',#6942,10.);
#1676=VECTOR('',#6943,10.);
#1677=VECTOR('',#6946,10.);
#1678=VECTOR('',#6947,10.);
#1679=VECTOR('',#6948,10.);
#1680=VECTOR('',#6951,10.);
#1681=VECTOR('',#6952,10.);
#1682=VECTOR('',#6957,10.);
#1683=VECTOR('',#6962,10.);
#1684=VECTOR('',#6963,10.);
#1685=VECTOR('',#6964,10.);
#1686=VECTOR('',#6965,10.);
#1687=VECTOR('',#6968,10.);
#1688=VECTOR('',#6969,10.);
#1689=VECTOR('',#6970,10.);
#1690=VECTOR('',#6973,10.);
#1691=VECTOR('',#6974,10.);
#1692=VECTOR('',#6979,10.);
#1693=VECTOR('',#6984,10.);
#1694=VECTOR('',#6985,10.);
#1695=VECTOR('',#6986,10.);
#1696=VECTOR('',#6987,10.);
#1697=VECTOR('',#6990,10.);
#1698=VECTOR('',#6991,10.);
#1699=VECTOR('',#6992,10.);
#1700=VECTOR('',#6995,9.99999999999999);
#1701=VECTOR('',#6996,9.99999999999999);
#1702=VECTOR('',#7001,10.);
#1703=VECTOR('',#7006,10.);
#1704=VECTOR('',#7007,10.);
#1705=VECTOR('',#7008,10.);
#1706=VECTOR('',#7009,10.);
#1707=VECTOR('',#7012,10.);
#1708=VECTOR('',#7013,10.);
#1709=VECTOR('',#7014,10.);
#1710=VECTOR('',#7017,10.);
#1711=VECTOR('',#7018,10.);
#1712=VECTOR('',#7019,10.);
#1713=VECTOR('',#7024,10.);
#1714=VECTOR('',#7031,10.);
#1715=VECTOR('',#7036,9.99999999999999);
#1716=VECTOR('',#7037,10.);
#1717=VECTOR('',#7038,9.99999999999999);
#1718=VECTOR('',#7039,10.);
#1719=VECTOR('',#7042,10.);
#1720=VECTOR('',#7043,10.);
#1721=VECTOR('',#7046,10.);
#1722=VECTOR('',#7047,10.);
#1723=VECTOR('',#7050,10.);
#1724=VECTOR('',#7051,10.);
#1725=VECTOR('',#7052,10.);
#1726=VECTOR('',#7053,10.);
#1727=VECTOR('',#7056,10.);
#1728=VECTOR('',#7057,10.);
#1729=VECTOR('',#7058,10.);
#1730=VECTOR('',#7061,10.);
#1731=VECTOR('',#7062,10.);
#1732=VECTOR('',#7067,10.);
#1733=VECTOR('',#7072,10.);
#1734=VECTOR('',#7073,10.);
#1735=VECTOR('',#7074,10.);
#1736=VECTOR('',#7075,10.);
#1737=VECTOR('',#7078,9.99999999999999);
#1738=VECTOR('',#7079,9.99999999999999);
#1739=VECTOR('',#7080,10.);
#1740=VECTOR('',#7083,10.);
#1741=VECTOR('',#7084,10.);
#1742=VECTOR('',#7085,10.);
#1743=VECTOR('',#7090,10.);
#1744=VECTOR('',#7097,10.);
#1745=VECTOR('',#7102,10.);
#1746=VECTOR('',#7103,10.);
#1747=VECTOR('',#7104,10.);
#1748=VECTOR('',#7105,10.);
#1749=VECTOR('',#7108,10.);
#1750=VECTOR('',#7109,10.);
#1751=VECTOR('',#7110,10.);
#1752=VECTOR('',#7113,9.99999999999999);
#1753=VECTOR('',#7114,10.);
#1754=VECTOR('',#7115,9.99999999999999);
#1755=VECTOR('',#7120,10.);
#1756=VECTOR('',#7127,10.);
#1757=VECTOR('',#7132,10.);
#1758=VECTOR('',#7133,10.);
#1759=VECTOR('',#7134,10.);
#1760=VECTOR('',#7135,10.);
#1761=VECTOR('',#7138,10.);
#1762=VECTOR('',#7139,10.);
#1763=VECTOR('',#7142,10.);
#1764=VECTOR('',#7143,10.);
#1765=VECTOR('',#7146,10.);
#1766=VECTOR('',#7147,10.);
#1767=VECTOR('',#7148,10.);
#1768=VECTOR('',#7149,10.);
#1769=VECTOR('',#7152,10.);
#1770=VECTOR('',#7153,10.);
#1771=VECTOR('',#7156,10.);
#1772=VECTOR('',#7157,10.);
#1773=VECTOR('',#7160,10.);
#1774=VECTOR('',#7161,10.);
#1775=VECTOR('',#7162,10.);
#1776=VECTOR('',#7163,10.);
#1777=VECTOR('',#7166,10.);
#1778=VECTOR('',#7167,10.);
#1779=VECTOR('',#7168,10.);
#1780=VECTOR('',#7171,10.);
#1781=VECTOR('',#7172,10.);
#1782=VECTOR('',#7177,10.);
#1783=VECTOR('',#7182,10.);
#1784=VECTOR('',#7183,10.);
#1785=VECTOR('',#7184,10.);
#1786=VECTOR('',#7185,10.);
#1787=VECTOR('',#7188,10.);
#1788=VECTOR('',#7189,10.);
#1789=VECTOR('',#7190,10.);
#1790=VECTOR('',#7193,10.);
#1791=VECTOR('',#7194,10.);
#1792=VECTOR('',#7199,10.);
#1793=VECTOR('',#7204,10.);
#1794=VECTOR('',#7205,10.);
#1795=VECTOR('',#7206,10.);
#1796=VECTOR('',#7207,10.);
#1797=VECTOR('',#7210,10.);
#1798=VECTOR('',#7211,10.);
#1799=VECTOR('',#7212,10.);
#1800=VECTOR('',#7215,10.);
#1801=VECTOR('',#7216,10.);
#1802=VECTOR('',#7217,10.);
#1803=VECTOR('',#7222,10.);
#1804=VECTOR('',#7229,10.);
#1805=VECTOR('',#7234,10.);
#1806=VECTOR('',#7235,10.);
#1807=VECTOR('',#7236,10.);
#1808=VECTOR('',#7237,10.);
#1809=VECTOR('',#7240,10.);
#1810=VECTOR('',#7241,10.);
#1811=VECTOR('',#7242,10.);
#1812=VECTOR('',#7245,10.);
#1813=VECTOR('',#7246,10.);
#1814=VECTOR('',#7251,10.);
#1815=VECTOR('',#7256,10.);
#1816=VECTOR('',#7257,10.);
#1817=VECTOR('',#7258,10.);
#1818=VECTOR('',#7259,10.);
#1819=VECTOR('',#7262,10.);
#1820=VECTOR('',#7263,10.);
#1821=VECTOR('',#7264,10.);
#1822=VECTOR('',#7267,10.);
#1823=VECTOR('',#7268,10.);
#1824=VECTOR('',#7273,10.);
#1825=VECTOR('',#7278,10.);
#1826=VECTOR('',#7279,10.);
#1827=VECTOR('',#7280,10.);
#1828=VECTOR('',#7281,10.);
#1829=VECTOR('',#7284,10.);
#1830=VECTOR('',#7285,10.);
#1831=VECTOR('',#7288,10.);
#1832=VECTOR('',#7289,10.);
#1833=VECTOR('',#7292,10.);
#1834=VECTOR('',#7293,10.);
#1835=VECTOR('',#7294,10.);
#1836=VECTOR('',#7295,10.);
#1837=VECTOR('',#7298,10.);
#1838=VECTOR('',#7299,10.);
#1839=VECTOR('',#7300,10.);
#1840=VECTOR('',#7303,10.);
#1841=VECTOR('',#7304,10.);
#1842=VECTOR('',#7305,10.);
#1843=VECTOR('',#7310,10.);
#1844=VECTOR('',#7317,10.);
#1845=VECTOR('',#7322,10.);
#1846=VECTOR('',#7323,10.);
#1847=VECTOR('',#7324,10.);
#1848=VECTOR('',#7325,10.);
#1849=VECTOR('',#7328,10.);
#1850=VECTOR('',#7329,10.);
#1851=VECTOR('',#7332,10.);
#1852=VECTOR('',#7333,10.);
#1853=VECTOR('',#7336,10.);
#1854=VECTOR('',#7337,10.);
#1855=VECTOR('',#7338,10.);
#1856=VECTOR('',#7339,10.);
#1857=VECTOR('',#7342,10.);
#1858=VECTOR('',#7343,10.);
#1859=VECTOR('',#7344,10.);
#1860=VECTOR('',#7347,10.);
#1861=VECTOR('',#7348,10.);
#1862=VECTOR('',#7349,10.);
#1863=VECTOR('',#7354,10.);
#1864=VECTOR('',#7361,10.);
#1865=VECTOR('',#7366,10.);
#1866=VECTOR('',#7367,10.);
#1867=VECTOR('',#7368,10.);
#1868=VECTOR('',#7369,10.);
#1869=VECTOR('',#7372,10.);
#1870=VECTOR('',#7373,10.);
#1871=VECTOR('',#7376,10.);
#1872=VECTOR('',#7377,10.);
#1873=VECTOR('',#7380,10.);
#1874=VECTOR('',#7381,10.);
#1875=VECTOR('',#7382,10.);
#1876=VECTOR('',#7383,10.);
#1877=VECTOR('',#7386,10.);
#1878=VECTOR('',#7387,10.);
#1879=VECTOR('',#7388,10.);
#1880=VECTOR('',#7391,10.);
#1881=VECTOR('',#7392,10.);
#1882=VECTOR('',#7393,10.);
#1883=VECTOR('',#7398,10.);
#1884=VECTOR('',#7405,10.);
#1885=VECTOR('',#7410,10.);
#1886=VECTOR('',#7411,10.);
#1887=VECTOR('',#7412,10.);
#1888=VECTOR('',#7413,10.);
#1889=VECTOR('',#7416,10.);
#1890=VECTOR('',#7417,10.);
#1891=VECTOR('',#7418,10.);
#1892=VECTOR('',#7421,10.);
#1893=VECTOR('',#7422,10.);
#1894=VECTOR('',#7427,10.);
#1895=VECTOR('',#7432,10.);
#1896=VECTOR('',#7433,10.);
#1897=VECTOR('',#7434,10.);
#1898=VECTOR('',#7435,10.);
#1899=VECTOR('',#7438,10.);
#1900=VECTOR('',#7439,10.);
#1901=VECTOR('',#7440,10.);
#1902=VECTOR('',#7443,10.);
#1903=VECTOR('',#7444,10.);
#1904=VECTOR('',#7449,10.);
#1905=VECTOR('',#7454,10.);
#1906=VECTOR('',#7455,10.);
#1907=VECTOR('',#7456,10.);
#1908=VECTOR('',#7457,10.);
#1909=VECTOR('',#7460,10.);
#1910=VECTOR('',#7461,10.);
#1911=VECTOR('',#7464,10.);
#1912=VECTOR('',#7465,10.);
#1913=VECTOR('',#7466,10.);
#1914=VECTOR('',#7471,10.);
#1915=VECTOR('',#7476,10.);
#1916=VECTOR('',#7477,10.);
#1917=VECTOR('',#7478,10.);
#1918=VECTOR('',#7479,10.);
#1919=VECTOR('',#7482,10.);
#1920=VECTOR('',#7483,10.);
#1921=VECTOR('',#7484,10.);
#1922=VECTOR('',#7487,10.);
#1923=VECTOR('',#7488,10.);
#1924=VECTOR('',#7489,10.);
#1925=VECTOR('',#7494,10.);
#1926=VECTOR('',#7501,10.);
#1927=VECTOR('',#7506,10.);
#1928=VECTOR('',#7507,10.);
#1929=VECTOR('',#7508,10.);
#1930=VECTOR('',#7509,10.);
#1931=VECTOR('',#7512,10.);
#1932=VECTOR('',#7513,10.);
#1933=VECTOR('',#7516,10.);
#1934=VECTOR('',#7517,10.);
#1935=VECTOR('',#7520,10.);
#1936=VECTOR('',#7521,10.);
#1937=VECTOR('',#7522,10.);
#1938=VECTOR('',#7523,10.);
#1939=VECTOR('',#7526,10.);
#1940=VECTOR('',#7527,10.);
#1941=VECTOR('',#7530,10.);
#1942=VECTOR('',#7531,10.);
#1943=VECTOR('',#7534,10.);
#1944=VECTOR('',#7535,10.);
#1945=VECTOR('',#7536,10.);
#1946=VECTOR('',#7537,10.);
#1947=VECTOR('',#7540,10.);
#1948=VECTOR('',#7541,10.);
#1949=VECTOR('',#7544,10.);
#1950=VECTOR('',#7545,10.);
#1951=VECTOR('',#7548,10.);
#1952=VECTOR('',#7549,10.);
#1953=VECTOR('',#7550,10.);
#1954=VECTOR('',#7551,10.);
#1955=VECTOR('',#7554,10.);
#1956=VECTOR('',#7555,10.);
#1957=VECTOR('',#7556,10.);
#1958=VECTOR('',#7557,10.);
#1959=VECTOR('',#7562,10.);
#1960=VECTOR('',#7569,10.);
#1961=VECTOR('',#7576,10.);
#1962=VECTOR('',#7583,10.);
#1963=VECTOR('',#7588,10.);
#1964=VECTOR('',#7589,10.);
#1965=VECTOR('',#7592,10.);
#1966=VECTOR('',#7593,10.);
#1967=VECTOR('',#7594,10.);
#1968=VECTOR('',#7595,10.);
#1969=VECTOR('',#7600,10.);
#1970=VECTOR('',#7607,10.);
#1971=VECTOR('',#7612,10.);
#1972=VECTOR('',#7613,10.);
#1973=VECTOR('',#7616,10.);
#1974=VECTOR('',#7617,10.);
#1975=VECTOR('',#7618,10.);
#1976=VECTOR('',#7619,10.);
#1977=VECTOR('',#7624,10.);
#1978=VECTOR('',#7631,10.);
#1979=VECTOR('',#7636,10.);
#1980=VECTOR('',#7637,10.);
#1981=VECTOR('',#7640,10.);
#1982=VECTOR('',#7641,10.);
#1983=VECTOR('',#7642,10.);
#1984=VECTOR('',#7643,10.);
#1985=VECTOR('',#7648,10.);
#1986=VECTOR('',#7655,10.);
#1987=VECTOR('',#7660,10.);
#1988=VECTOR('',#7661,10.);
#1989=VECTOR('',#7664,10.);
#1990=VECTOR('',#7665,10.);
#1991=VECTOR('',#7666,10.);
#1992=VECTOR('',#7667,10.);
#1993=VECTOR('',#7672,10.);
#1994=VECTOR('',#7679,10.);
#1995=VECTOR('',#7684,9.99999999999999);
#1996=VECTOR('',#7685,9.99999999999999);
#1997=VECTOR('',#7688,10.);
#1998=VECTOR('',#7689,10.);
#1999=VECTOR('',#7694,6.00000000000001);
#2000=VECTOR('',#7707,3.37715398312954);
#2001=VECTOR('',#7716,10.);
#2002=VECTOR('',#7717,10.);
#2003=VECTOR('',#7718,10.);
#2004=VECTOR('',#7721,10.);
#2005=VECTOR('',#7724,10.);
#2006=VECTOR('',#7727,10.);
#2007=VECTOR('',#7730,10.);
#2008=VECTOR('',#7731,10.);
#2009=VECTOR('',#7732,10.);
#2010=VECTOR('',#7735,10.);
#2011=VECTOR('',#7740,10.);
#2012=VECTOR('',#7741,10.);
#2013=VECTOR('',#7742,9.99999999999999);
#2014=VECTOR('',#7747,10.);
#2015=VECTOR('',#7748,10.);
#2016=VECTOR('',#7751,10.);
#2017=VECTOR('',#7752,10.);
#2018=VECTOR('',#7757,10.);
#2019=VECTOR('',#7760,10.);
#2020=VECTOR('',#7761,10.);
#2021=VECTOR('',#7764,10.);
#2022=VECTOR('',#7767,9.99999999999999);
#2023=VECTOR('',#7768,10.);
#2024=VECTOR('',#7771,10.);
#2025=VECTOR('',#7774,10.);
#2026=VECTOR('',#7777,10.);
#2027=VECTOR('',#7780,10.);
#2028=VECTOR('',#7785,10.);
#2029=VECTOR('',#7788,10.);
#2030=VECTOR('',#7791,6.00000000000001);
#2031=VECTOR('',#7794,10.);
#2032=VECTOR('',#7797,10.);
#2033=VECTOR('',#7800,10.);
#2034=VECTOR('',#7803,10.);
#2035=VECTOR('',#7806,10.);
#2036=VECTOR('',#7809,10.);
#2037=VECTOR('',#7812,10.);
#2038=VECTOR('',#7821,4.8);
#2039=VECTOR('',#7828,4.872);
#2040=VECTOR('',#7837,4.8);
#2041=VECTOR('',#7842,4.8);
#2042=VECTOR('',#7857,6.);
#2043=VECTOR('',#7866,4.845);
#2044=VECTOR('',#7881,3.1184375);
#2045=VECTOR('',#7888,3.1184375);
#2046=VECTOR('',#7901,3.272);
#2047=VECTOR('',#7914,3.1184375);
#2048=VECTOR('',#7919,3.0734375);
#2049=VECTOR('',#7932,2.);
#2050=VECTOR('',#7953,3.2);
#2051=VECTOR('',#7968,4.36638040039984);
#2052=VECTOR('',#7987,4.57071796769724);
#2053=VECTOR('',#8006,4.62071796769724);
#2054=VECTOR('',#8025,4.27977786002139);
#2055=VECTOR('',#8040,3.2);
#2056=VECTOR('',#8055,4.36638040039984);
#2057=VECTOR('',#8074,4.57071796769724);
#2058=VECTOR('',#8093,4.62071796769724);
#2059=VECTOR('',#8112,4.27977786002139);
#2060=CIRCLE('',#5722,4.8);
#2061=CIRCLE('',#5723,4.8);
#2062=CIRCLE('',#5725,4.872);
#2063=CIRCLE('',#5726,4.872);
#2064=CIRCLE('',#5728,4.8);
#2065=CIRCLE('',#5729,4.8);
#2066=CIRCLE('',#5730,4.8);
#2067=CIRCLE('',#5732,4.845);
#2068=CIRCLE('',#5734,6.);
#2069=CIRCLE('',#5735,0.2);
#2070=CIRCLE('',#5736,5.8);
#2071=CIRCLE('',#5738,6.);
#2072=CIRCLE('',#5740,5.8);
#2073=CIRCLE('',#5741,0.2);
#2074=CIRCLE('',#5743,4.845);
#2075=CIRCLE('',#5749,3.1184375);
#2076=CIRCLE('',#5750,3.0734375);
#2077=CIRCLE('',#5751,3.1184375);
#2078=CIRCLE('',#5753,3.1184375);
#2079=CIRCLE('',#5755,0.138976293103448);
#2080=CIRCLE('',#5756,3.2);
#2081=CIRCLE('',#5758,3.272);
#2082=CIRCLE('',#5759,3.272);
#2083=CIRCLE('',#5761,3.2);
#2084=CIRCLE('',#5762,0.138976293103448);
#2085=CIRCLE('',#5763,3.1184375);
#2086=CIRCLE('',#5765,3.1184375);
#2087=CIRCLE('',#5767,3.0734375);
#2088=CIRCLE('',#5769,2.2);
#2089=CIRCLE('',#5770,0.2);
#2090=CIRCLE('',#5771,2.);
#2091=CIRCLE('',#5773,2.);
#2092=CIRCLE('',#5775,0.2);
#2093=CIRCLE('',#5776,2.2);
#2094=CIRCLE('',#5782,3.2);
#2095=CIRCLE('',#5783,3.2);
#2096=CIRCLE('',#5785,4.22108058265378);
#2097=CIRCLE('',#5786,0.0900000000000005);
#2098=CIRCLE('',#5787,4.14313829631318);
#2099=CIRCLE('',#5789,4.36638040039984);
#2100=CIRCLE('',#5791,4.38370090847553);
#2101=CIRCLE('',#5792,0.0200000000000002);
#2102=CIRCLE('',#5794,4.64);
#2103=CIRCLE('',#5795,0.119999999999999);
#2104=CIRCLE('',#5796,4.58);
#2105=CIRCLE('',#5798,4.57071796769724);
#2106=CIRCLE('',#5800,4.39071796769724);
#2107=CIRCLE('',#5801,0.12);
#2108=CIRCLE('',#5803,4.62071796769724);
#2109=CIRCLE('',#5804,0.22);
#2110=CIRCLE('',#5805,4.29071796769724);
#2111=CIRCLE('',#5807,4.69);
#2112=CIRCLE('',#5809,4.58);
#2113=CIRCLE('',#5810,0.219999999999999);
#2114=CIRCLE('',#5812,4.27977786002139);
#2115=CIRCLE('',#5813,0.12);
#2116=CIRCLE('',#5814,4.38370090847553);
#2117=CIRCLE('',#5816,4.13736479362129);
#2118=CIRCLE('',#5823,3.2);
#2119=CIRCLE('',#5824,3.2);
#2120=CIRCLE('',#5826,4.22108058265378);
#2121=CIRCLE('',#5827,0.0900000000000005);
#2122=CIRCLE('',#5828,4.14313829631318);
#2123=CIRCLE('',#5830,4.36638040039984);
#2124=CIRCLE('',#5832,4.38370090847553);
#2125=CIRCLE('',#5833,0.0200000000000002);
#2126=CIRCLE('',#5835,4.64);
#2127=CIRCLE('',#5836,0.119999999999999);
#2128=CIRCLE('',#5837,4.58);
#2129=CIRCLE('',#5839,4.57071796769724);
#2130=CIRCLE('',#5841,4.39071796769724);
#2131=CIRCLE('',#5842,0.12);
#2132=CIRCLE('',#5844,4.62071796769724);
#2133=CIRCLE('',#5845,0.22);
#2134=CIRCLE('',#5846,4.29071796769724);
#2135=CIRCLE('',#5848,4.69);
#2136=CIRCLE('',#5850,4.58);
#2137=CIRCLE('',#5851,0.219999999999999);
#2138=CIRCLE('',#5853,4.27977786002139);
#2139=CIRCLE('',#5854,0.12);
#2140=CIRCLE('',#5855,4.38370090847553);
#2141=CIRCLE('',#5857,4.13736479362129);
#2142=CIRCLE('',#5865,1.954);
#2143=CIRCLE('',#5866,1.570585);
#2144=CIRCLE('',#5870,3.91587722848039);
#2145=CIRCLE('',#5871,3.91587722848039);
#2146=CIRCLE('',#5872,3.91587722848039);
#2147=CIRCLE('',#5874,2.32389732910985);
#2148=CIRCLE('',#5876,2.32389732910985);
#2149=CIRCLE('',#5878,3.91780884605665);
#2150=CIRCLE('',#5879,1.6);
#2151=CIRCLE('',#5881,4.);
#2152=CIRCLE('',#5884,1.78524999999977);
#2153=CIRCLE('',#5886,1.78525000000146);
#2154=CIRCLE('',#5888,1.954);
#2155=CIRCLE('',#5892,2.);
#2156=CIRCLE('',#5893,2.);
#2157=CIRCLE('',#5895,2.);
#2158=CIRCLE('',#5896,2.);
#2159=CIRCLE('',#5898,6.00000000000001);
#2160=CIRCLE('',#5899,6.00000000000001);
#2161=CIRCLE('',#5901,7.00000000000001);
#2162=CIRCLE('',#5902,7.00000000000001);
#2163=CIRCLE('',#5905,7.00000000000001);
#2164=CIRCLE('',#5907,6.00000000000001);
#2165=CIRCLE('',#5908,6.00000000000001);
#2166=CIRCLE('',#5910,7.00000000000001);
#2167=CIRCLE('',#5921,1.99999999999999);
#2168=CIRCLE('',#5922,1.99999999999999);
#2169=CIRCLE('',#5924,2.99999999999999);
#2170=CIRCLE('',#5925,2.99999999999999);
#2171=CIRCLE('',#5930,0.420000000000005);
#2172=CIRCLE('',#5931,0.35);
#2173=CIRCLE('',#5932,0.770000000000005);
#2174=CIRCLE('',#5933,0.770000000000005);
#2175=CIRCLE('',#5937,0.420000000000005);
#2176=CIRCLE('',#5938,0.35);
#2177=CIRCLE('',#5939,0.770000000000005);
#2178=CIRCLE('',#5940,0.770000000000005);
#2179=CIRCLE('',#5944,1.99999999999999);
#2180=CIRCLE('',#5946,1.99999999999999);
#2181=CIRCLE('',#5953,25.5);
#2182=CIRCLE('',#5954,25.5);
#2183=CIRCLE('',#5956,25.5);
#2184=CIRCLE('',#5957,25.5);
#2185=CIRCLE('',#5962,25.5);
#2186=CIRCLE('',#5963,25.5);
#2187=CIRCLE('',#5968,25.5);
#2188=CIRCLE('',#5969,25.5);
#2189=CIRCLE('',#5974,25.5);
#2190=CIRCLE('',#5975,25.5);
#2191=CIRCLE('',#5980,25.5);
#2192=CIRCLE('',#5981,25.5);
#2193=CIRCLE('',#5986,25.5);
#2194=CIRCLE('',#5987,25.5);
#2195=CIRCLE('',#5989,25.5);
#2196=CIRCLE('',#5990,25.5);
#2197=CIRCLE('',#5998,25.5);
#2198=CIRCLE('',#5999,25.5);
#2199=CIRCLE('',#6004,25.5);
#2200=CIRCLE('',#6005,25.5);
#2201=CIRCLE('',#6007,25.5);
#2202=CIRCLE('',#6008,25.5);
#2203=CIRCLE('',#6013,25.5);
#2204=CIRCLE('',#6014,25.5);
#2205=CIRCLE('',#6016,25.5);
#2206=CIRCLE('',#6017,25.5);
#2207=CIRCLE('',#6028,25.5);
#2208=CIRCLE('',#6029,25.5);
#2209=CIRCLE('',#6034,25.5);
#2210=CIRCLE('',#6035,25.5);
#2211=CIRCLE('',#6040,25.5);
#2212=CIRCLE('',#6041,25.5);
#2213=CIRCLE('',#6043,25.5);
#2214=CIRCLE('',#6044,25.5);
#2215=CIRCLE('',#6049,25.5);
#2216=CIRCLE('',#6050,25.5);
#2217=CIRCLE('',#6055,25.5);
#2218=CIRCLE('',#6056,25.5);
#2219=CIRCLE('',#6064,25.5);
#2220=CIRCLE('',#6065,25.5);
#2221=CIRCLE('',#6067,25.5);
#2222=CIRCLE('',#6068,25.5);
#2223=CIRCLE('',#6076,25.5);
#2224=CIRCLE('',#6077,25.5);
#2225=CIRCLE('',#6079,25.5);
#2226=CIRCLE('',#6080,25.5);
#2227=CIRCLE('',#6088,25.5);
#2228=CIRCLE('',#6089,25.5);
#2229=CIRCLE('',#6091,25.5);
#2230=CIRCLE('',#6092,25.5);
#2231=CIRCLE('',#6097,25.5);
#2232=CIRCLE('',#6098,25.5);
#2233=CIRCLE('',#6103,25.5);
#2234=CIRCLE('',#6104,25.5);
#2235=CIRCLE('',#6109,25.5);
#2236=CIRCLE('',#6110,25.5);
#2237=CIRCLE('',#6115,25.5);
#2238=CIRCLE('',#6116,25.5);
#2239=CIRCLE('',#6118,25.5);
#2240=CIRCLE('',#6119,25.5);
#2241=CIRCLE('',#6132,22.);
#2242=CIRCLE('',#6133,22.);
#2243=CIRCLE('',#6135,22.);
#2244=CIRCLE('',#6136,22.);
#2245=CIRCLE('',#6138,7.00000000000001);
#2246=CIRCLE('',#6139,7.00000000000001);
#2247=CIRCLE('',#6141,7.00000000000001);
#2248=CIRCLE('',#6142,7.00000000000001);
#2249=CIRCLE('',#6146,22.);
#2250=CIRCLE('',#6147,22.);
#2251=CIRCLE('',#6149,7.00000000000001);
#2252=CIRCLE('',#6150,7.00000000000001);
#2253=CIRCLE('',#6154,22.);
#2254=CIRCLE('',#6155,22.);
#2255=CIRCLE('',#6157,7.00000000000001);
#2256=CIRCLE('',#6158,7.00000000000001);
#2257=CIRCLE('',#6162,22.);
#2258=CIRCLE('',#6163,22.);
#2259=CIRCLE('',#6165,7.00000000000001);
#2260=CIRCLE('',#6166,7.00000000000001);
#2261=CIRCLE('',#6170,22.);
#2262=CIRCLE('',#6171,22.);
#2263=CIRCLE('',#6173,7.00000000000001);
#2264=CIRCLE('',#6174,7.00000000000001);
#2265=CIRCLE('',#6178,6.00000000000001);
#2266=CIRCLE('',#6179,6.00000000000001);
#2267=CIRCLE('',#6184,3.37715398312954);
#2268=CIRCLE('',#6185,3.37715398312954);
#2269=CIRCLE('',#6187,6.00000000000001);
#2270=CIRCLE('',#6189,7.00000000000001);
#2271=CIRCLE('',#6190,29.0155772121002);
#2272=CIRCLE('',#6191,32.2155772121002);
#2273=CIRCLE('',#6192,7.00000000000001);
#2274=CIRCLE('',#6193,26.714151341222);
#2275=CIRCLE('',#6194,23.514151341222);
#2276=CIRCLE('',#6197,26.714151341222);
#2277=CIRCLE('',#6200,23.514151341222);
#2278=CIRCLE('',#6204,7.00000000000001);
#2279=CIRCLE('',#6205,32.2155772121003);
#2280=CIRCLE('',#6206,29.0155772121003);
#2281=CIRCLE('',#6207,7.00000000000001);
#2282=CIRCLE('',#6208,6.00000000000001);
#2283=CIRCLE('',#6222,4.8);
#2284=CIRCLE('',#6223,4.8);
#2285=CIRCLE('',#6225,4.872);
#2286=CIRCLE('',#6226,4.872);
#2287=CIRCLE('',#6228,4.8);
#2288=CIRCLE('',#6229,4.8);
#2289=CIRCLE('',#6230,4.8);
#2290=CIRCLE('',#6232,4.845);
#2291=CIRCLE('',#6234,6.);
#2292=CIRCLE('',#6235,0.2);
#2293=CIRCLE('',#6236,5.8);
#2294=CIRCLE('',#6238,6.);
#2295=CIRCLE('',#6240,5.8);
#2296=CIRCLE('',#6241,0.2);
#2297=CIRCLE('',#6243,4.845);
#2298=CIRCLE('',#6249,3.1184375);
#2299=CIRCLE('',#6250,3.0734375);
#2300=CIRCLE('',#6251,3.1184375);
#2301=CIRCLE('',#6253,3.1184375);
#2302=CIRCLE('',#6255,0.138976293103448);
#2303=CIRCLE('',#6256,3.2);
#2304=CIRCLE('',#6258,3.272);
#2305=CIRCLE('',#6259,3.272);
#2306=CIRCLE('',#6261,3.2);
#2307=CIRCLE('',#6262,0.138976293103448);
#2308=CIRCLE('',#6263,3.1184375);
#2309=CIRCLE('',#6265,3.1184375);
#2310=CIRCLE('',#6267,3.0734375);
#2311=CIRCLE('',#6269,2.2);
#2312=CIRCLE('',#6270,0.2);
#2313=CIRCLE('',#6271,2.);
#2314=CIRCLE('',#6273,2.);
#2315=CIRCLE('',#6275,0.2);
#2316=CIRCLE('',#6276,2.2);
#2317=CIRCLE('',#6282,3.2);
#2318=CIRCLE('',#6283,3.2);
#2319=CIRCLE('',#6285,4.22108058265378);
#2320=CIRCLE('',#6286,0.0900000000000005);
#2321=CIRCLE('',#6287,4.14313829631318);
#2322=CIRCLE('',#6289,4.36638040039984);
#2323=CIRCLE('',#6291,4.38370090847553);
#2324=CIRCLE('',#6292,0.0200000000000002);
#2325=CIRCLE('',#6294,4.64);
#2326=CIRCLE('',#6295,0.119999999999999);
#2327=CIRCLE('',#6296,4.58);
#2328=CIRCLE('',#6298,4.57071796769724);
#2329=CIRCLE('',#6300,4.39071796769724);
#2330=CIRCLE('',#6301,0.12);
#2331=CIRCLE('',#6303,4.62071796769724);
#2332=CIRCLE('',#6304,0.22);
#2333=CIRCLE('',#6305,4.29071796769724);
#2334=CIRCLE('',#6307,4.69);
#2335=CIRCLE('',#6309,4.58);
#2336=CIRCLE('',#6310,0.219999999999999);
#2337=CIRCLE('',#6312,4.27977786002139);
#2338=CIRCLE('',#6313,0.12);
#2339=CIRCLE('',#6314,4.38370090847553);
#2340=CIRCLE('',#6316,4.13736479362129);
#2341=CIRCLE('',#6323,3.2);
#2342=CIRCLE('',#6324,3.2);
#2343=CIRCLE('',#6326,4.22108058265378);
#2344=CIRCLE('',#6327,0.0900000000000005);
#2345=CIRCLE('',#6328,4.14313829631318);
#2346=CIRCLE('',#6330,4.36638040039984);
#2347=CIRCLE('',#6332,4.38370090847553);
#2348=CIRCLE('',#6333,0.0200000000000002);
#2349=CIRCLE('',#6335,4.64);
#2350=CIRCLE('',#6336,0.119999999999999);
#2351=CIRCLE('',#6337,4.58);
#2352=CIRCLE('',#6339,4.57071796769724);
#2353=CIRCLE('',#6341,4.39071796769724);
#2354=CIRCLE('',#6342,0.12);
#2355=CIRCLE('',#6344,4.62071796769724);
#2356=CIRCLE('',#6345,0.22);
#2357=CIRCLE('',#6346,4.29071796769724);
#2358=CIRCLE('',#6348,4.69);
#2359=CIRCLE('',#6350,4.58);
#2360=CIRCLE('',#6351,0.219999999999999);
#2361=CIRCLE('',#6353,4.27977786002139);
#2362=CIRCLE('',#6354,0.12);
#2363=CIRCLE('',#6355,4.38370090847553);
#2364=CIRCLE('',#6357,4.13736479362129);
#2365=VERTEX_POINT('',#8142);
#2366=VERTEX_POINT('',#8144);
#2367=VERTEX_POINT('',#8148);
#2368=VERTEX_POINT('',#8150);
#2369=VERTEX_POINT('',#8154);
#2370=VERTEX_POINT('',#8155);
#2371=VERTEX_POINT('',#8158);
#2372=VERTEX_POINT('',#8162);
#2373=VERTEX_POINT('',#8166);
#2374=VERTEX_POINT('',#8168);
#2375=VERTEX_POINT('',#8172);
#2376=VERTEX_POINT('',#8176);
#2377=VERTEX_POINT('',#8180);
#2378=VERTEX_POINT('',#8188);
#2379=VERTEX_POINT('',#8189);
#2380=VERTEX_POINT('',#8191);
#2381=VERTEX_POINT('',#8196);
#2382=VERTEX_POINT('',#8200);
#2383=VERTEX_POINT('',#8204);
#2384=VERTEX_POINT('',#8206);
#2385=VERTEX_POINT('',#8210);
#2386=VERTEX_POINT('',#8212);
#2387=VERTEX_POINT('',#8216);
#2388=VERTEX_POINT('',#8220);
#2389=VERTEX_POINT('',#8224);
#2390=VERTEX_POINT('',#8226);
#2391=VERTEX_POINT('',#8230);
#2392=VERTEX_POINT('',#8234);
#2393=VERTEX_POINT('',#8242);
#2394=VERTEX_POINT('',#8244);
#2395=VERTEX_POINT('',#8248);
#2396=VERTEX_POINT('',#8250);
#2397=VERTEX_POINT('',#8254);
#2398=VERTEX_POINT('',#8258);
#2399=VERTEX_POINT('',#8262);
#2400=VERTEX_POINT('',#8264);
#2401=VERTEX_POINT('',#8268);
#2402=VERTEX_POINT('',#8272);
#2403=VERTEX_POINT('',#8276);
#2404=VERTEX_POINT('',#8278);
#2405=VERTEX_POINT('',#8282);
#2406=VERTEX_POINT('',#8286);
#2407=VERTEX_POINT('',#8290);
#2408=VERTEX_POINT('',#8292);
#2409=VERTEX_POINT('',#8296);
#2410=VERTEX_POINT('',#8305);
#2411=VERTEX_POINT('',#8307);
#2412=VERTEX_POINT('',#8311);
#2413=VERTEX_POINT('',#8313);
#2414=VERTEX_POINT('',#8317);
#2415=VERTEX_POINT('',#8321);
#2416=VERTEX_POINT('',#8325);
#2417=VERTEX_POINT('',#8327);
#2418=VERTEX_POINT('',#8331);
#2419=VERTEX_POINT('',#8335);
#2420=VERTEX_POINT('',#8339);
#2421=VERTEX_POINT('',#8341);
#2422=VERTEX_POINT('',#8345);
#2423=VERTEX_POINT('',#8349);
#2424=VERTEX_POINT('',#8353);
#2425=VERTEX_POINT('',#8355);
#2426=VERTEX_POINT('',#8359);
#2427=VERTEX_POINT('',#8369);
#2428=VERTEX_POINT('',#8371);
#2429=VERTEX_POINT('',#8375);
#2430=VERTEX_POINT('',#8376);
#2431=VERTEX_POINT('',#8387);
#2432=VERTEX_POINT('',#8389);
#2433=VERTEX_POINT('',#8402);
#2434=VERTEX_POINT('',#8403);
#2435=VERTEX_POINT('',#8414);
#2436=VERTEX_POINT('',#8416);
#2437=VERTEX_POINT('',#8430);
#2438=VERTEX_POINT('',#8438);
#2439=VERTEX_POINT('',#8442);
#2440=VERTEX_POINT('',#8447);
#2441=VERTEX_POINT('',#8450);
#2442=VERTEX_POINT('',#8454);
#2443=VERTEX_POINT('',#8461);
#2444=VERTEX_POINT('',#8463);
#2445=VERTEX_POINT('',#8467);
#2446=VERTEX_POINT('',#8469);
#2447=VERTEX_POINT('',#8473);
#2448=VERTEX_POINT('',#8475);
#2449=VERTEX_POINT('',#8479);
#2450=VERTEX_POINT('',#8481);
#2451=VERTEX_POINT('',#8486);
#2452=VERTEX_POINT('',#8487);
#2453=VERTEX_POINT('',#8489);
#2454=VERTEX_POINT('',#8491);
#2455=VERTEX_POINT('',#8494);
#2456=VERTEX_POINT('',#8497);
#2457=VERTEX_POINT('',#8499);
#2458=VERTEX_POINT('',#8503);
#2459=VERTEX_POINT('',#8509);
#2460=VERTEX_POINT('',#8511);
#2461=VERTEX_POINT('',#8515);
#2462=VERTEX_POINT('',#8519);
#2463=VERTEX_POINT('',#8528);
#2464=VERTEX_POINT('',#8530);
#2465=VERTEX_POINT('',#8534);
#2466=VERTEX_POINT('',#8536);
#2467=VERTEX_POINT('',#8543);
#2468=VERTEX_POINT('',#8545);
#2469=VERTEX_POINT('',#8547);
#2470=VERTEX_POINT('',#8551);
#2471=VERTEX_POINT('',#8553);
#2472=VERTEX_POINT('',#8592);
#2473=VERTEX_POINT('',#8594);
#2474=VERTEX_POINT('',#8596);
#2475=VERTEX_POINT('',#8600);
#2476=VERTEX_POINT('',#8601);
#2477=VERTEX_POINT('',#8612);
#2478=VERTEX_POINT('',#8644);
#2479=VERTEX_POINT('',#8647);
#2480=VERTEX_POINT('',#8654);
#2481=VERTEX_POINT('',#8655);
#2482=VERTEX_POINT('',#8657);
#2483=VERTEX_POINT('',#8659);
#2484=VERTEX_POINT('',#8663);
#2485=VERTEX_POINT('',#8665);
#2486=VERTEX_POINT('',#8669);
#2487=VERTEX_POINT('',#8671);
#2488=VERTEX_POINT('',#8675);
#2489=VERTEX_POINT('',#8677);
#2490=VERTEX_POINT('',#8681);
#2491=VERTEX_POINT('',#8683);
#2492=VERTEX_POINT('',#8687);
#2493=VERTEX_POINT('',#8688);
#2494=VERTEX_POINT('',#8690);
#2495=VERTEX_POINT('',#8692);
#2496=VERTEX_POINT('',#8696);
#2497=VERTEX_POINT('',#8698);
#2498=VERTEX_POINT('',#8705);
#2499=VERTEX_POINT('',#8707);
#2500=VERTEX_POINT('',#8711);
#2501=VERTEX_POINT('',#8712);
#2502=VERTEX_POINT('',#8714);
#2503=VERTEX_POINT('',#8716);
#2504=VERTEX_POINT('',#8720);
#2505=VERTEX_POINT('',#8722);
#2506=VERTEX_POINT('',#8729);
#2507=VERTEX_POINT('',#8731);
#2508=VERTEX_POINT('',#8735);
#2509=VERTEX_POINT('',#8736);
#2510=VERTEX_POINT('',#8738);
#2511=VERTEX_POINT('',#8740);
#2512=VERTEX_POINT('',#8744);
#2513=VERTEX_POINT('',#8746);
#2514=VERTEX_POINT('',#8753);
#2515=VERTEX_POINT('',#8755);
#2516=VERTEX_POINT('',#8759);
#2517=VERTEX_POINT('',#8760);
#2518=VERTEX_POINT('',#8762);
#2519=VERTEX_POINT('',#8764);
#2520=VERTEX_POINT('',#8768);
#2521=VERTEX_POINT('',#8770);
#2522=VERTEX_POINT('',#8777);
#2523=VERTEX_POINT('',#8779);
#2524=VERTEX_POINT('',#8783);
#2525=VERTEX_POINT('',#8784);
#2526=VERTEX_POINT('',#8786);
#2527=VERTEX_POINT('',#8788);
#2528=VERTEX_POINT('',#8792);
#2529=VERTEX_POINT('',#8794);
#2530=VERTEX_POINT('',#8798);
#2531=VERTEX_POINT('',#8800);
#2532=VERTEX_POINT('',#8804);
#2533=VERTEX_POINT('',#8806);
#2534=VERTEX_POINT('',#8810);
#2535=VERTEX_POINT('',#8812);
#2536=VERTEX_POINT('',#8816);
#2537=VERTEX_POINT('',#8817);
#2538=VERTEX_POINT('',#8819);
#2539=VERTEX_POINT('',#8821);
#2540=VERTEX_POINT('',#8831);
#2541=VERTEX_POINT('',#8832);
#2542=VERTEX_POINT('',#8834);
#2543=VERTEX_POINT('',#8836);
#2544=VERTEX_POINT('',#8840);
#2545=VERTEX_POINT('',#8842);
#2546=VERTEX_POINT('',#8849);
#2547=VERTEX_POINT('',#8851);
#2548=VERTEX_POINT('',#8855);
#2549=VERTEX_POINT('',#8856);
#2550=VERTEX_POINT('',#8858);
#2551=VERTEX_POINT('',#8860);
#2552=VERTEX_POINT('',#8864);
#2553=VERTEX_POINT('',#8866);
#2554=VERTEX_POINT('',#8870);
#2555=VERTEX_POINT('',#8872);
#2556=VERTEX_POINT('',#8876);
#2557=VERTEX_POINT('',#8878);
#2558=VERTEX_POINT('',#8882);
#2559=VERTEX_POINT('',#8884);
#2560=VERTEX_POINT('',#8888);
#2561=VERTEX_POINT('',#8889);
#2562=VERTEX_POINT('',#8891);
#2563=VERTEX_POINT('',#8893);
#2564=VERTEX_POINT('',#8897);
#2565=VERTEX_POINT('',#8899);
#2566=VERTEX_POINT('',#8903);
#2567=VERTEX_POINT('',#8905);
#2568=VERTEX_POINT('',#8909);
#2569=VERTEX_POINT('',#8911);
#2570=VERTEX_POINT('',#8915);
#2571=VERTEX_POINT('',#8917);
#2572=VERTEX_POINT('',#8921);
#2573=VERTEX_POINT('',#8922);
#2574=VERTEX_POINT('',#8924);
#2575=VERTEX_POINT('',#8926);
#2576=VERTEX_POINT('',#8936);
#2577=VERTEX_POINT('',#8937);
#2578=VERTEX_POINT('',#8939);
#2579=VERTEX_POINT('',#8941);
#2580=VERTEX_POINT('',#8951);
#2581=VERTEX_POINT('',#8952);
#2582=VERTEX_POINT('',#8954);
#2583=VERTEX_POINT('',#8956);
#2584=VERTEX_POINT('',#8960);
#2585=VERTEX_POINT('',#8962);
#2586=VERTEX_POINT('',#8969);
#2587=VERTEX_POINT('',#8971);
#2588=VERTEX_POINT('',#8975);
#2589=VERTEX_POINT('',#8976);
#2590=VERTEX_POINT('',#8978);
#2591=VERTEX_POINT('',#8980);
#2592=VERTEX_POINT('',#8984);
#2593=VERTEX_POINT('',#8986);
#2594=VERTEX_POINT('',#8993);
#2595=VERTEX_POINT('',#8995);
#2596=VERTEX_POINT('',#8999);
#2597=VERTEX_POINT('',#9000);
#2598=VERTEX_POINT('',#9002);
#2599=VERTEX_POINT('',#9004);
#2600=VERTEX_POINT('',#9008);
#2601=VERTEX_POINT('',#9010);
#2602=VERTEX_POINT('',#9014);
#2603=VERTEX_POINT('',#9016);
#2604=VERTEX_POINT('',#9020);
#2605=VERTEX_POINT('',#9022);
#2606=VERTEX_POINT('',#9026);
#2607=VERTEX_POINT('',#9028);
#2608=VERTEX_POINT('',#9032);
#2609=VERTEX_POINT('',#9033);
#2610=VERTEX_POINT('',#9035);
#2611=VERTEX_POINT('',#9037);
#2612=VERTEX_POINT('',#9041);
#2613=VERTEX_POINT('',#9043);
#2614=VERTEX_POINT('',#9050);
#2615=VERTEX_POINT('',#9052);
#2616=VERTEX_POINT('',#9056);
#2617=VERTEX_POINT('',#9057);
#2618=VERTEX_POINT('',#9059);
#2619=VERTEX_POINT('',#9061);
#2620=VERTEX_POINT('',#9065);
#2621=VERTEX_POINT('',#9067);
#2622=VERTEX_POINT('',#9074);
#2623=VERTEX_POINT('',#9076);
#2624=VERTEX_POINT('',#9080);
#2625=VERTEX_POINT('',#9081);
#2626=VERTEX_POINT('',#9083);
#2627=VERTEX_POINT('',#9085);
#2628=VERTEX_POINT('',#9095);
#2629=VERTEX_POINT('',#9096);
#2630=VERTEX_POINT('',#9098);
#2631=VERTEX_POINT('',#9100);
#2632=VERTEX_POINT('',#9104);
#2633=VERTEX_POINT('',#9106);
#2634=VERTEX_POINT('',#9110);
#2635=VERTEX_POINT('',#9112);
#2636=VERTEX_POINT('',#9116);
#2637=VERTEX_POINT('',#9118);
#2638=VERTEX_POINT('',#9122);
#2639=VERTEX_POINT('',#9124);
#2640=VERTEX_POINT('',#9128);
#2641=VERTEX_POINT('',#9129);
#2642=VERTEX_POINT('',#9131);
#2643=VERTEX_POINT('',#9133);
#2644=VERTEX_POINT('',#9143);
#2645=VERTEX_POINT('',#9144);
#2646=VERTEX_POINT('',#9146);
#2647=VERTEX_POINT('',#9148);
#2648=VERTEX_POINT('',#9152);
#2649=VERTEX_POINT('',#9154);
#2650=VERTEX_POINT('',#9158);
#2651=VERTEX_POINT('',#9160);
#2652=VERTEX_POINT('',#9164);
#2653=VERTEX_POINT('',#9166);
#2654=VERTEX_POINT('',#9170);
#2655=VERTEX_POINT('',#9172);
#2656=VERTEX_POINT('',#9176);
#2657=VERTEX_POINT('',#9177);
#2658=VERTEX_POINT('',#9179);
#2659=VERTEX_POINT('',#9181);
#2660=VERTEX_POINT('',#9191);
#2661=VERTEX_POINT('',#9192);
#2662=VERTEX_POINT('',#9194);
#2663=VERTEX_POINT('',#9196);
#2664=VERTEX_POINT('',#9200);
#2665=VERTEX_POINT('',#9202);
#2666=VERTEX_POINT('',#9206);
#2667=VERTEX_POINT('',#9208);
#2668=VERTEX_POINT('',#9212);
#2669=VERTEX_POINT('',#9214);
#2670=VERTEX_POINT('',#9218);
#2671=VERTEX_POINT('',#9220);
#2672=VERTEX_POINT('',#9224);
#2673=VERTEX_POINT('',#9225);
#2674=VERTEX_POINT('',#9227);
#2675=VERTEX_POINT('',#9229);
#2676=VERTEX_POINT('',#9233);
#2677=VERTEX_POINT('',#9235);
#2678=VERTEX_POINT('',#9242);
#2679=VERTEX_POINT('',#9244);
#2680=VERTEX_POINT('',#9248);
#2681=VERTEX_POINT('',#9249);
#2682=VERTEX_POINT('',#9251);
#2683=VERTEX_POINT('',#9253);
#2684=VERTEX_POINT('',#9257);
#2685=VERTEX_POINT('',#9259);
#2686=VERTEX_POINT('',#9266);
#2687=VERTEX_POINT('',#9268);
#2688=VERTEX_POINT('',#9272);
#2689=VERTEX_POINT('',#9273);
#2690=VERTEX_POINT('',#9275);
#2691=VERTEX_POINT('',#9277);
#2692=VERTEX_POINT('',#9284);
#2693=VERTEX_POINT('',#9286);
#2694=VERTEX_POINT('',#9290);
#2695=VERTEX_POINT('',#9292);
#2696=VERTEX_POINT('',#9296);
#2697=VERTEX_POINT('',#9297);
#2698=VERTEX_POINT('',#9299);
#2699=VERTEX_POINT('',#9301);
#2700=VERTEX_POINT('',#9305);
#2701=VERTEX_POINT('',#9307);
#2702=VERTEX_POINT('',#9311);
#2703=VERTEX_POINT('',#9313);
#2704=VERTEX_POINT('',#9317);
#2705=VERTEX_POINT('',#9319);
#2706=VERTEX_POINT('',#9323);
#2707=VERTEX_POINT('',#9325);
#2708=VERTEX_POINT('',#9329);
#2709=VERTEX_POINT('',#9330);
#2710=VERTEX_POINT('',#9332);
#2711=VERTEX_POINT('',#9334);
#2712=VERTEX_POINT('',#9344);
#2713=VERTEX_POINT('',#9345);
#2714=VERTEX_POINT('',#9347);
#2715=VERTEX_POINT('',#9349);
#2716=VERTEX_POINT('',#9359);
#2717=VERTEX_POINT('',#9360);
#2718=VERTEX_POINT('',#9362);
#2719=VERTEX_POINT('',#9364);
#2720=VERTEX_POINT('',#9374);
#2721=VERTEX_POINT('',#9375);
#2722=VERTEX_POINT('',#9377);
#2723=VERTEX_POINT('',#9379);
#2724=VERTEX_POINT('',#9383);
#2725=VERTEX_POINT('',#9384);
#2726=VERTEX_POINT('',#9386);
#2727=VERTEX_POINT('',#9388);
#2728=VERTEX_POINT('',#9392);
#2729=VERTEX_POINT('',#9394);
#2730=VERTEX_POINT('',#9398);
#2731=VERTEX_POINT('',#9400);
#2732=VERTEX_POINT('',#9404);
#2733=VERTEX_POINT('',#9406);
#2734=VERTEX_POINT('',#9410);
#2735=VERTEX_POINT('',#9412);
#2736=VERTEX_POINT('',#9419);
#2737=VERTEX_POINT('',#9420);
#2738=VERTEX_POINT('',#9422);
#2739=VERTEX_POINT('',#9424);
#2740=VERTEX_POINT('',#9428);
#2741=VERTEX_POINT('',#9430);
#2742=VERTEX_POINT('',#9434);
#2743=VERTEX_POINT('',#9436);
#2744=VERTEX_POINT('',#9443);
#2745=VERTEX_POINT('',#9444);
#2746=VERTEX_POINT('',#9446);
#2747=VERTEX_POINT('',#9448);
#2748=VERTEX_POINT('',#9452);
#2749=VERTEX_POINT('',#9454);
#2750=VERTEX_POINT('',#9458);
#2751=VERTEX_POINT('',#9460);
#2752=VERTEX_POINT('',#9467);
#2753=VERTEX_POINT('',#9468);
#2754=VERTEX_POINT('',#9470);
#2755=VERTEX_POINT('',#9472);
#2756=VERTEX_POINT('',#9476);
#2757=VERTEX_POINT('',#9478);
#2758=VERTEX_POINT('',#9482);
#2759=VERTEX_POINT('',#9484);
#2760=VERTEX_POINT('',#9491);
#2761=VERTEX_POINT('',#9492);
#2762=VERTEX_POINT('',#9494);
#2763=VERTEX_POINT('',#9496);
#2764=VERTEX_POINT('',#9500);
#2765=VERTEX_POINT('',#9502);
#2766=VERTEX_POINT('',#9506);
#2767=VERTEX_POINT('',#9508);
#2768=VERTEX_POINT('',#9518);
#2769=VERTEX_POINT('',#9520);
#2770=VERTEX_POINT('',#9527);
#2771=VERTEX_POINT('',#9529);
#2772=VERTEX_POINT('',#9533);
#2773=VERTEX_POINT('',#9536);
#2774=VERTEX_POINT('',#9537);
#2775=VERTEX_POINT('',#9539);
#2776=VERTEX_POINT('',#9541);
#2777=VERTEX_POINT('',#9543);
#2778=VERTEX_POINT('',#9545);
#2779=VERTEX_POINT('',#9547);
#2780=VERTEX_POINT('',#9549);
#2781=VERTEX_POINT('',#9551);
#2782=VERTEX_POINT('',#9553);
#2783=VERTEX_POINT('',#9555);
#2784=VERTEX_POINT('',#9557);
#2785=VERTEX_POINT('',#9559);
#2786=VERTEX_POINT('',#9561);
#2787=VERTEX_POINT('',#9563);
#2788=VERTEX_POINT('',#9565);
#2789=VERTEX_POINT('',#9569);
#2790=VERTEX_POINT('',#9571);
#2791=VERTEX_POINT('',#9575);
#2792=VERTEX_POINT('',#9576);
#2793=VERTEX_POINT('',#9581);
#2794=VERTEX_POINT('',#9585);
#2795=VERTEX_POINT('',#9589);
#2796=VERTEX_POINT('',#9595);
#2797=VERTEX_POINT('',#9597);
#2798=VERTEX_POINT('',#9599);
#2799=VERTEX_POINT('',#9601);
#2800=VERTEX_POINT('',#9603);
#2801=VERTEX_POINT('',#9605);
#2802=VERTEX_POINT('',#9607);
#2803=VERTEX_POINT('',#9609);
#2804=VERTEX_POINT('',#9611);
#2805=VERTEX_POINT('',#9614);
#2806=VERTEX_POINT('',#9639);
#2807=VERTEX_POINT('',#9641);
#2808=VERTEX_POINT('',#9645);
#2809=VERTEX_POINT('',#9647);
#2810=VERTEX_POINT('',#9651);
#2811=VERTEX_POINT('',#9652);
#2812=VERTEX_POINT('',#9655);
#2813=VERTEX_POINT('',#9659);
#2814=VERTEX_POINT('',#9663);
#2815=VERTEX_POINT('',#9665);
#2816=VERTEX_POINT('',#9669);
#2817=VERTEX_POINT('',#9673);
#2818=VERTEX_POINT('',#9677);
#2819=VERTEX_POINT('',#9685);
#2820=VERTEX_POINT('',#9686);
#2821=VERTEX_POINT('',#9688);
#2822=VERTEX_POINT('',#9693);
#2823=VERTEX_POINT('',#9697);
#2824=VERTEX_POINT('',#9701);
#2825=VERTEX_POINT('',#9703);
#2826=VERTEX_POINT('',#9707);
#2827=VERTEX_POINT('',#9709);
#2828=VERTEX_POINT('',#9713);
#2829=VERTEX_POINT('',#9717);
#2830=VERTEX_POINT('',#9721);
#2831=VERTEX_POINT('',#9723);
#2832=VERTEX_POINT('',#9727);
#2833=VERTEX_POINT('',#9731);
#2834=VERTEX_POINT('',#9739);
#2835=VERTEX_POINT('',#9741);
#2836=VERTEX_POINT('',#9745);
#2837=VERTEX_POINT('',#9747);
#2838=VERTEX_POINT('',#9751);
#2839=VERTEX_POINT('',#9755);
#2840=VERTEX_POINT('',#9759);
#2841=VERTEX_POINT('',#9761);
#2842=VERTEX_POINT('',#9765);
#2843=VERTEX_POINT('',#9769);
#2844=VERTEX_POINT('',#9773);
#2845=VERTEX_POINT('',#9775);
#2846=VERTEX_POINT('',#9779);
#2847=VERTEX_POINT('',#9783);
#2848=VERTEX_POINT('',#9787);
#2849=VERTEX_POINT('',#9789);
#2850=VERTEX_POINT('',#9793);
#2851=VERTEX_POINT('',#9802);
#2852=VERTEX_POINT('',#9804);
#2853=VERTEX_POINT('',#9808);
#2854=VERTEX_POINT('',#9810);
#2855=VERTEX_POINT('',#9814);
#2856=VERTEX_POINT('',#9818);
#2857=VERTEX_POINT('',#9822);
#2858=VERTEX_POINT('',#9824);
#2859=VERTEX_POINT('',#9828);
#2860=VERTEX_POINT('',#9832);
#2861=VERTEX_POINT('',#9836);
#2862=VERTEX_POINT('',#9838);
#2863=VERTEX_POINT('',#9842);
#2864=VERTEX_POINT('',#9846);
#2865=VERTEX_POINT('',#9850);
#2866=VERTEX_POINT('',#9852);
#2867=VERTEX_POINT('',#9856);
#2868=EDGE_CURVE('',#2365,#2365,#2060,.T.);
#2869=EDGE_CURVE('',#2365,#2366,#1132,.T.);
#2870=EDGE_CURVE('',#2366,#2366,#2061,.T.);
#2871=EDGE_CURVE('',#2367,#2367,#2062,.T.);
#2872=EDGE_CURVE('',#2367,#2368,#1133,.T.);
#2873=EDGE_CURVE('',#2368,#2368,#2063,.T.);
#2874=EDGE_CURVE('',#2369,#2370,#2064,.T.);
#2875=EDGE_CURVE('',#2370,#2369,#2065,.T.);
#2876=EDGE_CURVE('',#2370,#2371,#1134,.T.);
#2877=EDGE_CURVE('',#2371,#2371,#2066,.T.);
#2878=EDGE_CURVE('',#2369,#2372,#1135,.T.);
#2879=EDGE_CURVE('',#2372,#2372,#2067,.T.);
#2880=EDGE_CURVE('',#2373,#2373,#2068,.T.);
#2881=EDGE_CURVE('',#2373,#2374,#2069,.T.);
#2882=EDGE_CURVE('',#2374,#2374,#2070,.T.);
#2883=EDGE_CURVE('',#2375,#2375,#2071,.T.);
#2884=EDGE_CURVE('',#2375,#2373,#1136,.T.);
#2885=EDGE_CURVE('',#2376,#2376,#2072,.T.);
#2886=EDGE_CURVE('',#2376,#2375,#2073,.T.);
#2887=EDGE_CURVE('',#2366,#2377,#1137,.T.);
#2888=EDGE_CURVE('',#2377,#2377,#2074,.T.);
#2889=EDGE_CURVE('',#2378,#2379,#2075,.T.);
#2890=EDGE_CURVE('',#2379,#2380,#1138,.T.);
#2891=EDGE_CURVE('',#2380,#2380,#2076,.T.);
#2892=EDGE_CURVE('',#2379,#2378,#2077,.T.);
#2893=EDGE_CURVE('',#2378,#2381,#1139,.T.);
#2894=EDGE_CURVE('',#2381,#2381,#2078,.T.);
#2895=EDGE_CURVE('',#2381,#2382,#2079,.T.);
#2896=EDGE_CURVE('',#2382,#2382,#2080,.T.);
#2897=EDGE_CURVE('',#2383,#2383,#2081,.T.);
#2898=EDGE_CURVE('',#2383,#2384,#1140,.T.);
#2899=EDGE_CURVE('',#2384,#2384,#2082,.T.);
#2900=EDGE_CURVE('',#2385,#2385,#2083,.T.);
#2901=EDGE_CURVE('',#2385,#2386,#2084,.T.);
#2902=EDGE_CURVE('',#2386,#2386,#2085,.T.);
#2903=EDGE_CURVE('',#2386,#2387,#1141,.T.);
#2904=EDGE_CURVE('',#2387,#2387,#2086,.T.);
#2905=EDGE_CURVE('',#2387,#2388,#1142,.T.);
#2906=EDGE_CURVE('',#2388,#2388,#2087,.T.);
#2907=EDGE_CURVE('',#2389,#2389,#2088,.T.);
#2908=EDGE_CURVE('',#2389,#2390,#2089,.T.);
#2909=EDGE_CURVE('',#2390,#2390,#2090,.T.);
#2910=EDGE_CURVE('',#2390,#2391,#1143,.T.);
#2911=EDGE_CURVE('',#2391,#2391,#2091,.T.);
#2912=EDGE_CURVE('',#2391,#2392,#2092,.T.);
#2913=EDGE_CURVE('',#2392,#2392,#2093,.T.);
#2914=EDGE_CURVE('',#2393,#2393,#2094,.T.);
#2915=EDGE_CURVE('',#2393,#2394,#1144,.T.);
#2916=EDGE_CURVE('',#2394,#2394,#2095,.T.);
#2917=EDGE_CURVE('',#2395,#2395,#2096,.T.);
#2918=EDGE_CURVE('',#2395,#2396,#2097,.T.);
#2919=EDGE_CURVE('',#2396,#2396,#2098,.T.);
#2920=EDGE_CURVE('',#2397,#2397,#2099,.T.);
#2921=EDGE_CURVE('',#2397,#2395,#1145,.T.);
#2922=EDGE_CURVE('',#2398,#2398,#2100,.T.);
#2923=EDGE_CURVE('',#2398,#2397,#2101,.T.);
#2924=EDGE_CURVE('',#2399,#2399,#2102,.T.);
#2925=EDGE_CURVE('',#2399,#2400,#2103,.T.);
#2926=EDGE_CURVE('',#2400,#2400,#2104,.T.);
#2927=EDGE_CURVE('',#2401,#2401,#2105,.T.);
#2928=EDGE_CURVE('',#2401,#2399,#1146,.T.);
#2929=EDGE_CURVE('',#2402,#2402,#2106,.T.);
#2930=EDGE_CURVE('',#2402,#2401,#2107,.T.);
#2931=EDGE_CURVE('',#2403,#2403,#2108,.T.);
#2932=EDGE_CURVE('',#2403,#2404,#2109,.T.);
#2933=EDGE_CURVE('',#2404,#2404,#2110,.T.);
#2934=EDGE_CURVE('',#2405,#2405,#2111,.T.);
#2935=EDGE_CURVE('',#2405,#2403,#1147,.T.);
#2936=EDGE_CURVE('',#2406,#2406,#2112,.T.);
#2937=EDGE_CURVE('',#2406,#2405,#2113,.T.);
#2938=EDGE_CURVE('',#2407,#2407,#2114,.T.);
#2939=EDGE_CURVE('',#2407,#2408,#2115,.T.);
#2940=EDGE_CURVE('',#2408,#2408,#2116,.T.);
#2941=EDGE_CURVE('',#2409,#2409,#2117,.T.);
#2942=EDGE_CURVE('',#2409,#2407,#1148,.T.);
#2943=EDGE_CURVE('',#2410,#2410,#2118,.T.);
#2944=EDGE_CURVE('',#2410,#2411,#1149,.T.);
#2945=EDGE_CURVE('',#2411,#2411,#2119,.T.);
#2946=EDGE_CURVE('',#2412,#2412,#2120,.T.);
#2947=EDGE_CURVE('',#2412,#2413,#2121,.T.);
#2948=EDGE_CURVE('',#2413,#2413,#2122,.T.);
#2949=EDGE_CURVE('',#2414,#2414,#2123,.T.);
#2950=EDGE_CURVE('',#2414,#2412,#1150,.T.);
#2951=EDGE_CURVE('',#2415,#2415,#2124,.T.);
#2952=EDGE_CURVE('',#2415,#2414,#2125,.T.);
#2953=EDGE_CURVE('',#2416,#2416,#2126,.T.);
#2954=EDGE_CURVE('',#2416,#2417,#2127,.T.);
#2955=EDGE_CURVE('',#2417,#2417,#2128,.T.);
#2956=EDGE_CURVE('',#2418,#2418,#2129,.T.);
#2957=EDGE_CURVE('',#2418,#2416,#1151,.T.);
#2958=EDGE_CURVE('',#2419,#2419,#2130,.T.);
#2959=EDGE_CURVE('',#2419,#2418,#2131,.T.);
#2960=EDGE_CURVE('',#2420,#2420,#2132,.T.);
#2961=EDGE_CURVE('',#2420,#2421,#2133,.T.);
#2962=EDGE_CURVE('',#2421,#2421,#2134,.T.);
#2963=EDGE_CURVE('',#2422,#2422,#2135,.T.);
#2964=EDGE_CURVE('',#2422,#2420,#1152,.T.);
#2965=EDGE_CURVE('',#2423,#2423,#2136,.T.);
#2966=EDGE_CURVE('',#2423,#2422,#2137,.T.);
#2967=EDGE_CURVE('',#2424,#2424,#2138,.T.);
#2968=EDGE_CURVE('',#2424,#2425,#2139,.T.);
#2969=EDGE_CURVE('',#2425,#2425,#2140,.T.);
#2970=EDGE_CURVE('',#2426,#2426,#2141,.T.);
#2971=EDGE_CURVE('',#2426,#2424,#1153,.T.);
#2972=EDGE_CURVE('',#2427,#2427,#2142,.T.);
#2973=EDGE_CURVE('',#2427,#2428,#1154,.T.);
#2974=EDGE_CURVE('',#2428,#2428,#2143,.T.);
#2975=EDGE_CURVE('',#2429,#2430,#43,.T.);
#2976=EDGE_CURVE('',#2429,#2431,#1155,.T.);
#2977=EDGE_CURVE('',#2432,#2431,#44,.T.);
#2978=EDGE_CURVE('',#2430,#2432,#1156,.T.);
#2979=EDGE_CURVE('',#2433,#2434,#45,.T.);
#2980=EDGE_CURVE('',#2435,#2433,#1157,.T.);
#2981=EDGE_CURVE('',#2436,#2435,#46,.T.);
#2982=EDGE_CURVE('',#2436,#2434,#1158,.T.);
#2983=EDGE_CURVE('',#2434,#2429,#2144,.T.);
#2984=EDGE_CURVE('',#2437,#2436,#2145,.T.);
#2985=EDGE_CURVE('',#2431,#2437,#2146,.T.);
#2986=EDGE_CURVE('',#2435,#2433,#2147,.T.);
#2987=EDGE_CURVE('',#2430,#2432,#2148,.T.);
#2988=EDGE_CURVE('',#2438,#2438,#2149,.T.);
#2989=EDGE_CURVE('',#2438,#2437,#2150,.T.);
#2990=EDGE_CURVE('',#2439,#2439,#2151,.T.);
#2991=EDGE_CURVE('',#2439,#2438,#1159,.T.);
#2992=EDGE_CURVE('',#2440,#2440,#2152,.T.);
#2993=EDGE_CURVE('',#2441,#2441,#2153,.T.);
#2994=EDGE_CURVE('',#2441,#2440,#1160,.T.);
#2995=EDGE_CURVE('',#2442,#2442,#2154,.T.);
#2996=EDGE_CURVE('',#2442,#2441,#1161,.T.);
#2997=EDGE_CURVE('',#2427,#2442,#1162,.T.);
#2998=EDGE_CURVE('',#2443,#2443,#2155,.T.);
#2999=EDGE_CURVE('',#2443,#2444,#1163,.T.);
#3000=EDGE_CURVE('',#2444,#2444,#2156,.T.);
#3001=EDGE_CURVE('',#2445,#2445,#2157,.T.);
#3002=EDGE_CURVE('',#2445,#2446,#1164,.T.);
#3003=EDGE_CURVE('',#2446,#2446,#2158,.T.);
#3004=EDGE_CURVE('',#2447,#2447,#2159,.T.);
#3005=EDGE_CURVE('',#2447,#2448,#1165,.T.);
#3006=EDGE_CURVE('',#2448,#2448,#2160,.T.);
#3007=EDGE_CURVE('',#2449,#2449,#2161,.T.);
#3008=EDGE_CURVE('',#2449,#2450,#1166,.T.);
#3009=EDGE_CURVE('',#2450,#2450,#2162,.T.);
#3010=EDGE_CURVE('',#2451,#2452,#1167,.T.);
#3011=EDGE_CURVE('',#2453,#2451,#1168,.T.);
#3012=EDGE_CURVE('',#2454,#2453,#1169,.T.);
#3013=EDGE_CURVE('',#2452,#2454,#1170,.T.);
#3014=EDGE_CURVE('',#2455,#2455,#2163,.T.);
#3015=EDGE_CURVE('',#2456,#2456,#2164,.T.);
#3016=EDGE_CURVE('',#2456,#2457,#1171,.T.);
#3017=EDGE_CURVE('',#2457,#2457,#2165,.T.);
#3018=EDGE_CURVE('',#2458,#2458,#2166,.T.);
#3019=EDGE_CURVE('',#2458,#2455,#1172,.T.);
#3020=EDGE_CURVE('',#2451,#2459,#1173,.T.);
#3021=EDGE_CURVE('',#2460,#2459,#1174,.T.);
#3022=EDGE_CURVE('',#2453,#2460,#1175,.T.);
#3023=EDGE_CURVE('',#2461,#2460,#1176,.T.);
#3024=EDGE_CURVE('',#2454,#2461,#1177,.T.);
#3025=EDGE_CURVE('',#2462,#2461,#1178,.T.);
#3026=EDGE_CURVE('',#2452,#2462,#1179,.T.);
#3027=EDGE_CURVE('',#2459,#2462,#1180,.T.);
#3028=EDGE_CURVE('',#2463,#2463,#2167,.T.);
#3029=EDGE_CURVE('',#2463,#2464,#1181,.T.);
#3030=EDGE_CURVE('',#2464,#2464,#2168,.T.);
#3031=EDGE_CURVE('',#2465,#2465,#2169,.T.);
#3032=EDGE_CURVE('',#2465,#2466,#1182,.T.);
#3033=EDGE_CURVE('',#2466,#2466,#2170,.T.);
#3034=EDGE_CURVE('',#2467,#2467,#2171,.T.);
#3035=EDGE_CURVE('',#2467,#2468,#2172,.T.);
#3036=EDGE_CURVE('',#2468,#2469,#2173,.T.);
#3037=EDGE_CURVE('',#2469,#2468,#2174,.T.);
#3038=EDGE_CURVE('',#2469,#2470,#1183,.T.);
#3039=EDGE_CURVE('',#2471,#2470,#47,.T.);
#3040=EDGE_CURVE('',#2470,#2471,#48,.T.);
#3041=EDGE_CURVE('',#2472,#2472,#2175,.T.);
#3042=EDGE_CURVE('',#2472,#2473,#2176,.T.);
#3043=EDGE_CURVE('',#2473,#2474,#2177,.T.);
#3044=EDGE_CURVE('',#2474,#2473,#2178,.T.);
#3045=EDGE_CURVE('',#2475,#2476,#49,.T.);
#3046=EDGE_CURVE('',#2477,#2475,#50,.T.);
#3047=EDGE_CURVE('',#2476,#2477,#51,.T.);
#3048=EDGE_CURVE('',#2476,#2474,#1184,.T.);
#3049=EDGE_CURVE('',#2478,#2478,#2179,.T.);
#3050=EDGE_CURVE('',#2479,#2479,#2180,.T.);
#3051=EDGE_CURVE('',#2479,#2476,#1185,.T.);
#3052=EDGE_CURVE('',#2477,#2478,#1186,.T.);
#3053=EDGE_CURVE('',#2480,#2481,#1187,.T.);
#3054=EDGE_CURVE('',#2480,#2482,#1188,.T.);
#3055=EDGE_CURVE('',#2483,#2482,#1189,.T.);
#3056=EDGE_CURVE('',#2481,#2483,#1190,.T.);
#3057=EDGE_CURVE('',#2481,#2484,#1191,.T.);
#3058=EDGE_CURVE('',#2485,#2483,#1192,.T.);
#3059=EDGE_CURVE('',#2484,#2485,#1193,.T.);
#3060=EDGE_CURVE('',#2480,#2486,#1194,.T.);
#3061=EDGE_CURVE('',#2487,#2486,#1195,.T.);
#3062=EDGE_CURVE('',#2482,#2487,#1196,.T.);
#3063=EDGE_CURVE('',#2488,#2485,#2181,.T.);
#3064=EDGE_CURVE('',#2488,#2489,#1197,.T.);
#3065=EDGE_CURVE('',#2489,#2484,#2182,.T.);
#3066=EDGE_CURVE('',#2486,#2490,#2183,.T.);
#3067=EDGE_CURVE('',#2490,#2491,#1198,.T.);
#3068=EDGE_CURVE('',#2487,#2491,#2184,.T.);
#3069=EDGE_CURVE('',#2492,#2493,#1199,.T.);
#3070=EDGE_CURVE('',#2492,#2494,#1200,.T.);
#3071=EDGE_CURVE('',#2495,#2494,#1201,.T.);
#3072=EDGE_CURVE('',#2493,#2495,#1202,.T.);
#3073=EDGE_CURVE('',#2493,#2496,#1203,.T.);
#3074=EDGE_CURVE('',#2497,#2495,#1204,.T.);
#3075=EDGE_CURVE('',#2496,#2497,#1205,.T.);
#3076=EDGE_CURVE('',#2492,#2489,#1206,.T.);
#3077=EDGE_CURVE('',#2494,#2488,#1207,.T.);
#3078=EDGE_CURVE('',#2498,#2497,#2185,.T.);
#3079=EDGE_CURVE('',#2498,#2499,#1208,.T.);
#3080=EDGE_CURVE('',#2499,#2496,#2186,.T.);
#3081=EDGE_CURVE('',#2500,#2501,#1209,.T.);
#3082=EDGE_CURVE('',#2500,#2502,#1210,.T.);
#3083=EDGE_CURVE('',#2503,#2502,#1211,.T.);
#3084=EDGE_CURVE('',#2501,#2503,#1212,.T.);
#3085=EDGE_CURVE('',#2501,#2504,#1213,.T.);
#3086=EDGE_CURVE('',#2505,#2503,#1214,.T.);
#3087=EDGE_CURVE('',#2504,#2505,#1215,.T.);
#3088=EDGE_CURVE('',#2500,#2499,#1216,.T.);
#3089=EDGE_CURVE('',#2502,#2498,#1217,.T.);
#3090=EDGE_CURVE('',#2506,#2505,#2187,.T.);
#3091=EDGE_CURVE('',#2506,#2507,#1218,.T.);
#3092=EDGE_CURVE('',#2507,#2504,#2188,.T.);
#3093=EDGE_CURVE('',#2508,#2509,#1219,.T.);
#3094=EDGE_CURVE('',#2508,#2510,#1220,.T.);
#3095=EDGE_CURVE('',#2511,#2510,#1221,.T.);
#3096=EDGE_CURVE('',#2509,#2511,#1222,.T.);
#3097=EDGE_CURVE('',#2509,#2512,#1223,.T.);
#3098=EDGE_CURVE('',#2513,#2511,#1224,.T.);
#3099=EDGE_CURVE('',#2512,#2513,#1225,.T.);
#3100=EDGE_CURVE('',#2508,#2507,#1226,.T.);
#3101=EDGE_CURVE('',#2510,#2506,#1227,.T.);
#3102=EDGE_CURVE('',#2514,#2513,#2189,.T.);
#3103=EDGE_CURVE('',#2514,#2515,#1228,.T.);
#3104=EDGE_CURVE('',#2515,#2512,#2190,.T.);
#3105=EDGE_CURVE('',#2516,#2517,#1229,.T.);
#3106=EDGE_CURVE('',#2516,#2518,#1230,.T.);
#3107=EDGE_CURVE('',#2519,#2518,#1231,.T.);
#3108=EDGE_CURVE('',#2517,#2519,#1232,.T.);
#3109=EDGE_CURVE('',#2517,#2520,#1233,.T.);
#3110=EDGE_CURVE('',#2521,#2519,#1234,.T.);
#3111=EDGE_CURVE('',#2520,#2521,#1235,.T.);
#3112=EDGE_CURVE('',#2516,#2515,#1236,.T.);
#3113=EDGE_CURVE('',#2518,#2514,#1237,.T.);
#3114=EDGE_CURVE('',#2522,#2521,#2191,.T.);
#3115=EDGE_CURVE('',#2522,#2523,#1238,.T.);
#3116=EDGE_CURVE('',#2523,#2520,#2192,.T.);
#3117=EDGE_CURVE('',#2524,#2525,#1239,.T.);
#3118=EDGE_CURVE('',#2524,#2526,#1240,.T.);
#3119=EDGE_CURVE('',#2527,#2526,#1241,.T.);
#3120=EDGE_CURVE('',#2525,#2527,#1242,.T.);
#3121=EDGE_CURVE('',#2525,#2528,#1243,.T.);
#3122=EDGE_CURVE('',#2529,#2527,#1244,.T.);
#3123=EDGE_CURVE('',#2528,#2529,#1245,.T.);
#3124=EDGE_CURVE('',#2524,#2530,#1246,.T.);
#3125=EDGE_CURVE('',#2531,#2530,#1247,.T.);
#3126=EDGE_CURVE('',#2526,#2531,#1248,.T.);
#3127=EDGE_CURVE('',#2532,#2529,#2193,.T.);
#3128=EDGE_CURVE('',#2532,#2533,#1249,.T.);
#3129=EDGE_CURVE('',#2533,#2528,#2194,.T.);
#3130=EDGE_CURVE('',#2530,#2534,#2195,.T.);
#3131=EDGE_CURVE('',#2534,#2535,#1250,.T.);
#3132=EDGE_CURVE('',#2531,#2535,#2196,.T.);
#3133=EDGE_CURVE('',#2536,#2537,#1251,.T.);
#3134=EDGE_CURVE('',#2536,#2538,#1252,.T.);
#3135=EDGE_CURVE('',#2539,#2538,#1253,.T.);
#3136=EDGE_CURVE('',#2537,#2539,#1254,.T.);
#3137=EDGE_CURVE('',#2537,#2534,#1255,.T.);
#3138=EDGE_CURVE('',#2535,#2539,#1256,.T.);
#3139=EDGE_CURVE('',#2536,#2523,#1257,.T.);
#3140=EDGE_CURVE('',#2538,#2522,#1258,.T.);
#3141=EDGE_CURVE('',#2540,#2541,#1259,.T.);
#3142=EDGE_CURVE('',#2540,#2542,#1260,.T.);
#3143=EDGE_CURVE('',#2543,#2542,#1261,.T.);
#3144=EDGE_CURVE('',#2541,#2543,#1262,.T.);
#3145=EDGE_CURVE('',#2541,#2544,#1263,.T.);
#3146=EDGE_CURVE('',#2545,#2543,#1264,.T.);
#3147=EDGE_CURVE('',#2544,#2545,#1265,.T.);
#3148=EDGE_CURVE('',#2540,#2533,#1266,.T.);
#3149=EDGE_CURVE('',#2542,#2532,#1267,.T.);
#3150=EDGE_CURVE('',#2546,#2545,#2197,.T.);
#3151=EDGE_CURVE('',#2546,#2547,#1268,.T.);
#3152=EDGE_CURVE('',#2547,#2544,#2198,.T.);
#3153=EDGE_CURVE('',#2548,#2549,#1269,.T.);
#3154=EDGE_CURVE('',#2548,#2550,#1270,.T.);
#3155=EDGE_CURVE('',#2551,#2550,#1271,.T.);
#3156=EDGE_CURVE('',#2549,#2551,#1272,.T.);
#3157=EDGE_CURVE('',#2549,#2552,#1273,.T.);
#3158=EDGE_CURVE('',#2553,#2551,#1274,.T.);
#3159=EDGE_CURVE('',#2552,#2553,#1275,.T.);
#3160=EDGE_CURVE('',#2548,#2554,#1276,.T.);
#3161=EDGE_CURVE('',#2555,#2554,#1277,.T.);
#3162=EDGE_CURVE('',#2550,#2555,#1278,.T.);
#3163=EDGE_CURVE('',#2556,#2553,#2199,.T.);
#3164=EDGE_CURVE('',#2556,#2557,#1279,.T.);
#3165=EDGE_CURVE('',#2557,#2552,#2200,.T.);
#3166=EDGE_CURVE('',#2554,#2558,#2201,.T.);
#3167=EDGE_CURVE('',#2558,#2559,#1280,.T.);
#3168=EDGE_CURVE('',#2555,#2559,#2202,.T.);
#3169=EDGE_CURVE('',#2560,#2561,#1281,.T.);
#3170=EDGE_CURVE('',#2560,#2562,#1282,.T.);
#3171=EDGE_CURVE('',#2563,#2562,#1283,.T.);
#3172=EDGE_CURVE('',#2561,#2563,#1284,.T.);
#3173=EDGE_CURVE('',#2561,#2564,#1285,.T.);
#3174=EDGE_CURVE('',#2565,#2563,#1286,.T.);
#3175=EDGE_CURVE('',#2564,#2565,#1287,.T.);
#3176=EDGE_CURVE('',#2560,#2566,#1288,.T.);
#3177=EDGE_CURVE('',#2567,#2566,#1289,.T.);
#3178=EDGE_CURVE('',#2562,#2567,#1290,.T.);
#3179=EDGE_CURVE('',#2568,#2565,#2203,.T.);
#3180=EDGE_CURVE('',#2568,#2569,#1291,.T.);
#3181=EDGE_CURVE('',#2569,#2564,#2204,.T.);
#3182=EDGE_CURVE('',#2566,#2570,#2205,.T.);
#3183=EDGE_CURVE('',#2570,#2571,#1292,.T.);
#3184=EDGE_CURVE('',#2567,#2571,#2206,.T.);
#3185=EDGE_CURVE('',#2572,#2573,#1293,.T.);
#3186=EDGE_CURVE('',#2572,#2574,#1294,.T.);
#3187=EDGE_CURVE('',#2575,#2574,#1295,.T.);
#3188=EDGE_CURVE('',#2573,#2575,#1296,.T.);
#3189=EDGE_CURVE('',#2573,#2570,#1297,.T.);
#3190=EDGE_CURVE('',#2571,#2575,#1298,.T.);
#3191=EDGE_CURVE('',#2572,#2557,#1299,.T.);
#3192=EDGE_CURVE('',#2574,#2556,#1300,.T.);
#3193=EDGE_CURVE('',#2576,#2577,#1301,.T.);
#3194=EDGE_CURVE('',#2576,#2578,#1302,.T.);
#3195=EDGE_CURVE('',#2579,#2578,#1303,.T.);
#3196=EDGE_CURVE('',#2577,#2579,#1304,.T.);
#3197=EDGE_CURVE('',#2577,#2558,#1305,.T.);
#3198=EDGE_CURVE('',#2559,#2579,#1306,.T.);
#3199=EDGE_CURVE('',#2576,#2547,#1307,.T.);
#3200=EDGE_CURVE('',#2578,#2546,#1308,.T.);
#3201=EDGE_CURVE('',#2580,#2581,#1309,.T.);
#3202=EDGE_CURVE('',#2580,#2582,#1310,.T.);
#3203=EDGE_CURVE('',#2583,#2582,#1311,.T.);
#3204=EDGE_CURVE('',#2581,#2583,#1312,.T.);
#3205=EDGE_CURVE('',#2581,#2584,#1313,.T.);
#3206=EDGE_CURVE('',#2585,#2583,#1314,.T.);
#3207=EDGE_CURVE('',#2584,#2585,#1315,.T.);
#3208=EDGE_CURVE('',#2580,#2569,#1316,.T.);
#3209=EDGE_CURVE('',#2582,#2568,#1317,.T.);
#3210=EDGE_CURVE('',#2586,#2585,#2207,.T.);
#3211=EDGE_CURVE('',#2586,#2587,#1318,.T.);
#3212=EDGE_CURVE('',#2587,#2584,#2208,.T.);
#3213=EDGE_CURVE('',#2588,#2589,#1319,.T.);
#3214=EDGE_CURVE('',#2588,#2590,#1320,.T.);
#3215=EDGE_CURVE('',#2591,#2590,#1321,.T.);
#3216=EDGE_CURVE('',#2589,#2591,#1322,.T.);
#3217=EDGE_CURVE('',#2589,#2592,#1323,.T.);
#3218=EDGE_CURVE('',#2593,#2591,#1324,.T.);
#3219=EDGE_CURVE('',#2592,#2593,#1325,.T.);
#3220=EDGE_CURVE('',#2588,#2587,#1326,.T.);
#3221=EDGE_CURVE('',#2590,#2586,#1327,.T.);
#3222=EDGE_CURVE('',#2594,#2593,#2209,.T.);
#3223=EDGE_CURVE('',#2594,#2595,#1328,.T.);
#3224=EDGE_CURVE('',#2595,#2592,#2210,.T.);
#3225=EDGE_CURVE('',#2596,#2597,#1329,.T.);
#3226=EDGE_CURVE('',#2596,#2598,#1330,.T.);
#3227=EDGE_CURVE('',#2599,#2598,#1331,.T.);
#3228=EDGE_CURVE('',#2597,#2599,#1332,.T.);
#3229=EDGE_CURVE('',#2597,#2600,#1333,.T.);
#3230=EDGE_CURVE('',#2601,#2599,#1334,.T.);
#3231=EDGE_CURVE('',#2600,#2601,#1335,.T.);
#3232=EDGE_CURVE('',#2596,#2602,#1336,.T.);
#3233=EDGE_CURVE('',#2603,#2602,#1337,.T.);
#3234=EDGE_CURVE('',#2598,#2603,#1338,.T.);
#3235=EDGE_CURVE('',#2604,#2601,#2211,.T.);
#3236=EDGE_CURVE('',#2604,#2605,#1339,.T.);
#3237=EDGE_CURVE('',#2605,#2600,#2212,.T.);
#3238=EDGE_CURVE('',#2602,#2606,#2213,.T.);
#3239=EDGE_CURVE('',#2606,#2607,#1340,.T.);
#3240=EDGE_CURVE('',#2603,#2607,#2214,.T.);
#3241=EDGE_CURVE('',#2608,#2609,#1341,.T.);
#3242=EDGE_CURVE('',#2608,#2610,#1342,.T.);
#3243=EDGE_CURVE('',#2611,#2610,#1343,.T.);
#3244=EDGE_CURVE('',#2609,#2611,#1344,.T.);
#3245=EDGE_CURVE('',#2609,#2612,#1345,.T.);
#3246=EDGE_CURVE('',#2613,#2611,#1346,.T.);
#3247=EDGE_CURVE('',#2612,#2613,#1347,.T.);
#3248=EDGE_CURVE('',#2608,#2595,#1348,.T.);
#3249=EDGE_CURVE('',#2610,#2594,#1349,.T.);
#3250=EDGE_CURVE('',#2614,#2613,#2215,.T.);
#3251=EDGE_CURVE('',#2614,#2615,#1350,.T.);
#3252=EDGE_CURVE('',#2615,#2612,#2216,.T.);
#3253=EDGE_CURVE('',#2616,#2617,#1351,.T.);
#3254=EDGE_CURVE('',#2616,#2618,#1352,.T.);
#3255=EDGE_CURVE('',#2619,#2618,#1353,.T.);
#3256=EDGE_CURVE('',#2617,#2619,#1354,.T.);
#3257=EDGE_CURVE('',#2617,#2620,#1355,.T.);
#3258=EDGE_CURVE('',#2621,#2619,#1356,.T.);
#3259=EDGE_CURVE('',#2620,#2621,#1357,.T.);
#3260=EDGE_CURVE('',#2616,#2615,#1358,.T.);
#3261=EDGE_CURVE('',#2618,#2614,#1359,.T.);
#3262=EDGE_CURVE('',#2622,#2621,#2217,.T.);
#3263=EDGE_CURVE('',#2622,#2623,#1360,.T.);
#3264=EDGE_CURVE('',#2623,#2620,#2218,.T.);
#3265=EDGE_CURVE('',#2624,#2625,#1361,.T.);
#3266=EDGE_CURVE('',#2624,#2626,#1362,.T.);
#3267=EDGE_CURVE('',#2627,#2626,#1363,.T.);
#3268=EDGE_CURVE('',#2625,#2627,#1364,.T.);
#3269=EDGE_CURVE('',#2625,#2606,#1365,.T.);
#3270=EDGE_CURVE('',#2607,#2627,#1366,.T.);
#3271=EDGE_CURVE('',#2624,#2623,#1367,.T.);
#3272=EDGE_CURVE('',#2626,#2622,#1368,.T.);
#3273=EDGE_CURVE('',#2628,#2629,#1369,.T.);
#3274=EDGE_CURVE('',#2628,#2630,#1370,.T.);
#3275=EDGE_CURVE('',#2631,#2630,#1371,.T.);
#3276=EDGE_CURVE('',#2629,#2631,#1372,.T.);
#3277=EDGE_CURVE('',#2629,#2632,#1373,.T.);
#3278=EDGE_CURVE('',#2633,#2631,#1374,.T.);
#3279=EDGE_CURVE('',#2632,#2633,#1375,.T.);
#3280=EDGE_CURVE('',#2628,#2634,#1376,.T.);
#3281=EDGE_CURVE('',#2635,#2634,#1377,.T.);
#3282=EDGE_CURVE('',#2630,#2635,#1378,.T.);
#3283=EDGE_CURVE('',#2636,#2633,#2219,.T.);
#3284=EDGE_CURVE('',#2636,#2637,#1379,.T.);
#3285=EDGE_CURVE('',#2637,#2632,#2220,.T.);
#3286=EDGE_CURVE('',#2634,#2638,#2221,.T.);
#3287=EDGE_CURVE('',#2638,#2639,#1380,.T.);
#3288=EDGE_CURVE('',#2635,#2639,#2222,.T.);
#3289=EDGE_CURVE('',#2640,#2641,#1381,.T.);
#3290=EDGE_CURVE('',#2640,#2642,#1382,.T.);
#3291=EDGE_CURVE('',#2643,#2642,#1383,.T.);
#3292=EDGE_CURVE('',#2641,#2643,#1384,.T.);
#3293=EDGE_CURVE('',#2641,#2638,#1385,.T.);
#3294=EDGE_CURVE('',#2639,#2643,#1386,.T.);
#3295=EDGE_CURVE('',#2640,#2605,#1387,.T.);
#3296=EDGE_CURVE('',#2642,#2604,#1388,.T.);
#3297=EDGE_CURVE('',#2644,#2645,#1389,.T.);
#3298=EDGE_CURVE('',#2644,#2646,#1390,.T.);
#3299=EDGE_CURVE('',#2647,#2646,#1391,.T.);
#3300=EDGE_CURVE('',#2645,#2647,#1392,.T.);
#3301=EDGE_CURVE('',#2645,#2648,#1393,.T.);
#3302=EDGE_CURVE('',#2649,#2647,#1394,.T.);
#3303=EDGE_CURVE('',#2648,#2649,#1395,.T.);
#3304=EDGE_CURVE('',#2644,#2650,#1396,.T.);
#3305=EDGE_CURVE('',#2651,#2650,#1397,.T.);
#3306=EDGE_CURVE('',#2646,#2651,#1398,.T.);
#3307=EDGE_CURVE('',#2652,#2649,#2223,.T.);
#3308=EDGE_CURVE('',#2652,#2653,#1399,.T.);
#3309=EDGE_CURVE('',#2653,#2648,#2224,.T.);
#3310=EDGE_CURVE('',#2650,#2654,#2225,.T.);
#3311=EDGE_CURVE('',#2654,#2655,#1400,.T.);
#3312=EDGE_CURVE('',#2651,#2655,#2226,.T.);
#3313=EDGE_CURVE('',#2656,#2657,#1401,.T.);
#3314=EDGE_CURVE('',#2656,#2658,#1402,.T.);
#3315=EDGE_CURVE('',#2659,#2658,#1403,.T.);
#3316=EDGE_CURVE('',#2657,#2659,#1404,.T.);
#3317=EDGE_CURVE('',#2657,#2490,#1405,.T.);
#3318=EDGE_CURVE('',#2491,#2659,#1406,.T.);
#3319=EDGE_CURVE('',#2656,#2653,#1407,.T.);
#3320=EDGE_CURVE('',#2658,#2652,#1408,.T.);
#3321=EDGE_CURVE('',#2660,#2661,#1409,.T.);
#3322=EDGE_CURVE('',#2660,#2662,#1410,.T.);
#3323=EDGE_CURVE('',#2663,#2662,#1411,.T.);
#3324=EDGE_CURVE('',#2661,#2663,#1412,.T.);
#3325=EDGE_CURVE('',#2661,#2664,#1413,.T.);
#3326=EDGE_CURVE('',#2665,#2663,#1414,.T.);
#3327=EDGE_CURVE('',#2664,#2665,#1415,.T.);
#3328=EDGE_CURVE('',#2660,#2666,#1416,.T.);
#3329=EDGE_CURVE('',#2667,#2666,#1417,.T.);
#3330=EDGE_CURVE('',#2662,#2667,#1418,.T.);
#3331=EDGE_CURVE('',#2668,#2665,#2227,.T.);
#3332=EDGE_CURVE('',#2668,#2669,#1419,.T.);
#3333=EDGE_CURVE('',#2669,#2664,#2228,.T.);
#3334=EDGE_CURVE('',#2666,#2670,#2229,.T.);
#3335=EDGE_CURVE('',#2670,#2671,#1420,.T.);
#3336=EDGE_CURVE('',#2667,#2671,#2230,.T.);
#3337=EDGE_CURVE('',#2672,#2673,#1421,.T.);
#3338=EDGE_CURVE('',#2672,#2674,#1422,.T.);
#3339=EDGE_CURVE('',#2675,#2674,#1423,.T.);
#3340=EDGE_CURVE('',#2673,#2675,#1424,.T.);
#3341=EDGE_CURVE('',#2673,#2676,#1425,.T.);
#3342=EDGE_CURVE('',#2677,#2675,#1426,.T.);
#3343=EDGE_CURVE('',#2676,#2677,#1427,.T.);
#3344=EDGE_CURVE('',#2672,#2669,#1428,.T.);
#3345=EDGE_CURVE('',#2674,#2668,#1429,.T.);
#3346=EDGE_CURVE('',#2678,#2677,#2231,.T.);
#3347=EDGE_CURVE('',#2678,#2679,#1430,.T.);
#3348=EDGE_CURVE('',#2679,#2676,#2232,.T.);
#3349=EDGE_CURVE('',#2680,#2681,#1431,.T.);
#3350=EDGE_CURVE('',#2680,#2682,#1432,.T.);
#3351=EDGE_CURVE('',#2683,#2682,#1433,.T.);
#3352=EDGE_CURVE('',#2681,#2683,#1434,.T.);
#3353=EDGE_CURVE('',#2681,#2684,#1435,.T.);
#3354=EDGE_CURVE('',#2685,#2683,#1436,.T.);
#3355=EDGE_CURVE('',#2684,#2685,#1437,.T.);
#3356=EDGE_CURVE('',#2680,#2679,#1438,.T.);
#3357=EDGE_CURVE('',#2682,#2678,#1439,.T.);
#3358=EDGE_CURVE('',#2686,#2685,#2233,.T.);
#3359=EDGE_CURVE('',#2686,#2687,#1440,.T.);
#3360=EDGE_CURVE('',#2687,#2684,#2234,.T.);
#3361=EDGE_CURVE('',#2688,#2689,#1441,.T.);
#3362=EDGE_CURVE('',#2688,#2690,#1442,.T.);
#3363=EDGE_CURVE('',#2691,#2690,#1443,.T.);
#3364=EDGE_CURVE('',#2689,#2691,#1444,.T.);
#3365=EDGE_CURVE('',#2689,#2670,#1445,.T.);
#3366=EDGE_CURVE('',#2671,#2691,#1446,.T.);
#3367=EDGE_CURVE('',#2688,#2692,#1447,.T.);
#3368=EDGE_CURVE('',#2693,#2692,#1448,.T.);
#3369=EDGE_CURVE('',#2690,#2693,#1449,.T.);
#3370=EDGE_CURVE('',#2692,#2694,#2235,.T.);
#3371=EDGE_CURVE('',#2694,#2695,#1450,.T.);
#3372=EDGE_CURVE('',#2693,#2695,#2236,.T.);
#3373=EDGE_CURVE('',#2696,#2697,#1451,.T.);
#3374=EDGE_CURVE('',#2696,#2698,#1452,.T.);
#3375=EDGE_CURVE('',#2699,#2698,#1453,.T.);
#3376=EDGE_CURVE('',#2697,#2699,#1454,.T.);
#3377=EDGE_CURVE('',#2697,#2700,#1455,.T.);
#3378=EDGE_CURVE('',#2701,#2699,#1456,.T.);
#3379=EDGE_CURVE('',#2700,#2701,#1457,.T.);
#3380=EDGE_CURVE('',#2696,#2702,#1458,.T.);
#3381=EDGE_CURVE('',#2703,#2702,#1459,.T.);
#3382=EDGE_CURVE('',#2698,#2703,#1460,.T.);
#3383=EDGE_CURVE('',#2704,#2701,#2237,.T.);
#3384=EDGE_CURVE('',#2704,#2705,#1461,.T.);
#3385=EDGE_CURVE('',#2705,#2700,#2238,.T.);
#3386=EDGE_CURVE('',#2702,#2706,#2239,.T.);
#3387=EDGE_CURVE('',#2706,#2707,#1462,.T.);
#3388=EDGE_CURVE('',#2703,#2707,#2240,.T.);
#3389=EDGE_CURVE('',#2708,#2709,#1463,.T.);
#3390=EDGE_CURVE('',#2708,#2710,#1464,.T.);
#3391=EDGE_CURVE('',#2711,#2710,#1465,.T.);
#3392=EDGE_CURVE('',#2709,#2711,#1466,.T.);
#3393=EDGE_CURVE('',#2709,#2694,#1467,.T.);
#3394=EDGE_CURVE('',#2695,#2711,#1468,.T.);
#3395=EDGE_CURVE('',#2708,#2705,#1469,.T.);
#3396=EDGE_CURVE('',#2710,#2704,#1470,.T.);
#3397=EDGE_CURVE('',#2712,#2713,#1471,.T.);
#3398=EDGE_CURVE('',#2712,#2714,#1472,.T.);
#3399=EDGE_CURVE('',#2715,#2714,#1473,.T.);
#3400=EDGE_CURVE('',#2713,#2715,#1474,.T.);
#3401=EDGE_CURVE('',#2713,#2706,#1475,.T.);
#3402=EDGE_CURVE('',#2707,#2715,#1476,.T.);
#3403=EDGE_CURVE('',#2712,#2637,#1477,.T.);
#3404=EDGE_CURVE('',#2714,#2636,#1478,.T.);
#3405=EDGE_CURVE('',#2716,#2717,#1479,.T.);
#3406=EDGE_CURVE('',#2716,#2718,#1480,.T.);
#3407=EDGE_CURVE('',#2719,#2718,#1481,.T.);
#3408=EDGE_CURVE('',#2717,#2719,#1482,.T.);
#3409=EDGE_CURVE('',#2717,#2654,#1483,.T.);
#3410=EDGE_CURVE('',#2655,#2719,#1484,.T.);
#3411=EDGE_CURVE('',#2716,#2687,#1485,.T.);
#3412=EDGE_CURVE('',#2718,#2686,#1486,.T.);
#3413=EDGE_CURVE('',#2720,#2721,#1487,.T.);
#3414=EDGE_CURVE('',#2722,#2720,#1488,.T.);
#3415=EDGE_CURVE('',#2723,#2722,#1489,.T.);
#3416=EDGE_CURVE('',#2721,#2723,#1490,.T.);
#3417=EDGE_CURVE('',#2724,#2725,#1491,.T.);
#3418=EDGE_CURVE('',#2726,#2725,#1492,.T.);
#3419=EDGE_CURVE('',#2727,#2726,#1493,.T.);
#3420=EDGE_CURVE('',#2724,#2727,#1494,.T.);
#3421=EDGE_CURVE('',#2728,#2723,#2241,.T.);
#3422=EDGE_CURVE('',#2728,#2729,#1495,.T.);
#3423=EDGE_CURVE('',#2729,#2721,#2242,.T.);
#3424=EDGE_CURVE('',#2725,#2730,#2243,.T.);
#3425=EDGE_CURVE('',#2730,#2731,#1496,.T.);
#3426=EDGE_CURVE('',#2726,#2731,#2244,.T.);
#3427=EDGE_CURVE('',#2732,#2727,#2245,.T.);
#3428=EDGE_CURVE('',#2732,#2733,#1497,.T.);
#3429=EDGE_CURVE('',#2733,#2724,#2246,.T.);
#3430=EDGE_CURVE('',#2720,#2734,#2247,.T.);
#3431=EDGE_CURVE('',#2734,#2735,#1498,.T.);
#3432=EDGE_CURVE('',#2722,#2735,#2248,.T.);
#3433=EDGE_CURVE('',#2733,#2730,#1499,.T.);
#3434=EDGE_CURVE('',#2731,#2732,#1500,.T.);
#3435=EDGE_CURVE('',#2736,#2737,#1501,.T.);
#3436=EDGE_CURVE('',#2738,#2737,#1502,.T.);
#3437=EDGE_CURVE('',#2739,#2738,#1503,.T.);
#3438=EDGE_CURVE('',#2736,#2739,#1504,.T.);
#3439=EDGE_CURVE('',#2737,#2740,#2249,.T.);
#3440=EDGE_CURVE('',#2740,#2741,#1505,.T.);
#3441=EDGE_CURVE('',#2738,#2741,#2250,.T.);
#3442=EDGE_CURVE('',#2742,#2739,#2251,.T.);
#3443=EDGE_CURVE('',#2742,#2743,#1506,.T.);
#3444=EDGE_CURVE('',#2743,#2736,#2252,.T.);
#3445=EDGE_CURVE('',#2743,#2740,#1507,.T.);
#3446=EDGE_CURVE('',#2741,#2742,#1508,.T.);
#3447=EDGE_CURVE('',#2744,#2745,#1509,.T.);
#3448=EDGE_CURVE('',#2746,#2745,#1510,.T.);
#3449=EDGE_CURVE('',#2747,#2746,#1511,.T.);
#3450=EDGE_CURVE('',#2744,#2747,#1512,.T.);
#3451=EDGE_CURVE('',#2745,#2748,#2253,.T.);
#3452=EDGE_CURVE('',#2748,#2749,#1513,.T.);
#3453=EDGE_CURVE('',#2746,#2749,#2254,.T.);
#3454=EDGE_CURVE('',#2750,#2747,#2255,.T.);
#3455=EDGE_CURVE('',#2750,#2751,#1514,.T.);
#3456=EDGE_CURVE('',#2751,#2744,#2256,.T.);
#3457=EDGE_CURVE('',#2751,#2748,#1515,.T.);
#3458=EDGE_CURVE('',#2749,#2750,#1516,.T.);
#3459=EDGE_CURVE('',#2752,#2753,#1517,.T.);
#3460=EDGE_CURVE('',#2754,#2753,#1518,.T.);
#3461=EDGE_CURVE('',#2755,#2754,#1519,.T.);
#3462=EDGE_CURVE('',#2752,#2755,#1520,.T.);
#3463=EDGE_CURVE('',#2753,#2756,#2257,.T.);
#3464=EDGE_CURVE('',#2756,#2757,#1521,.T.);
#3465=EDGE_CURVE('',#2754,#2757,#2258,.T.);
#3466=EDGE_CURVE('',#2758,#2755,#2259,.T.);
#3467=EDGE_CURVE('',#2758,#2759,#1522,.T.);
#3468=EDGE_CURVE('',#2759,#2752,#2260,.T.);
#3469=EDGE_CURVE('',#2759,#2756,#1523,.T.);
#3470=EDGE_CURVE('',#2757,#2758,#1524,.T.);
#3471=EDGE_CURVE('',#2760,#2761,#1525,.T.);
#3472=EDGE_CURVE('',#2762,#2761,#1526,.T.);
#3473=EDGE_CURVE('',#2763,#2762,#1527,.T.);
#3474=EDGE_CURVE('',#2760,#2763,#1528,.T.);
#3475=EDGE_CURVE('',#2761,#2764,#2261,.T.);
#3476=EDGE_CURVE('',#2764,#2765,#1529,.T.);
#3477=EDGE_CURVE('',#2762,#2765,#2262,.T.);
#3478=EDGE_CURVE('',#2766,#2763,#2263,.T.);
#3479=EDGE_CURVE('',#2766,#2767,#1530,.T.);
#3480=EDGE_CURVE('',#2767,#2760,#2264,.T.);
#3481=EDGE_CURVE('',#2767,#2764,#1531,.T.);
#3482=EDGE_CURVE('',#2765,#2766,#1532,.T.);
#3483=EDGE_CURVE('',#2734,#2729,#1533,.T.);
#3484=EDGE_CURVE('',#2735,#2728,#1534,.T.);
#3485=EDGE_CURVE('',#2768,#2768,#2265,.T.);
#3486=EDGE_CURVE('',#2768,#2769,#1535,.T.);
#3487=EDGE_CURVE('',#2769,#2769,#2266,.T.);
#3488=EDGE_CURVE('',#2770,#2770,#2267,.F.);
#3489=EDGE_CURVE('',#2770,#2771,#1536,.T.);
#3490=EDGE_CURVE('',#2771,#2771,#2268,.T.);
#3491=EDGE_CURVE('',#2772,#2772,#2269,.T.);
#3492=EDGE_CURVE('',#2773,#2774,#1537,.T.);
#3493=EDGE_CURVE('',#2774,#2775,#1538,.T.);
#3494=EDGE_CURVE('',#2775,#2776,#1539,.T.);
#3495=EDGE_CURVE('',#2776,#2777,#2270,.T.);
#3496=EDGE_CURVE('',#2777,#2778,#1540,.T.);
#3497=EDGE_CURVE('',#2778,#2779,#2271,.T.);
#3498=EDGE_CURVE('',#2779,#2780,#1541,.T.);
#3499=EDGE_CURVE('',#2780,#2781,#2272,.T.);
#3500=EDGE_CURVE('',#2781,#2782,#1542,.T.);
#3501=EDGE_CURVE('',#2782,#2783,#2273,.T.);
#3502=EDGE_CURVE('',#2783,#2784,#1543,.T.);
#3503=EDGE_CURVE('',#2784,#2785,#1544,.T.);
#3504=EDGE_CURVE('',#2785,#2786,#1545,.T.);
#3505=EDGE_CURVE('',#2786,#2787,#2274,.T.);
#3506=EDGE_CURVE('',#2787,#2788,#1546,.T.);
#3507=EDGE_CURVE('',#2788,#2773,#2275,.T.);
#3508=EDGE_CURVE('',#2775,#2789,#1547,.T.);
#3509=EDGE_CURVE('',#2774,#2790,#1548,.T.);
#3510=EDGE_CURVE('',#2790,#2789,#1549,.T.);
#3511=EDGE_CURVE('',#2791,#2792,#2276,.T.);
#3512=EDGE_CURVE('',#2792,#2787,#1550,.T.);
#3513=EDGE_CURVE('',#2791,#2786,#1551,.T.);
#3514=EDGE_CURVE('',#2792,#2793,#1552,.T.);
#3515=EDGE_CURVE('',#2793,#2788,#1553,.T.);
#3516=EDGE_CURVE('',#2794,#2793,#2277,.T.);
#3517=EDGE_CURVE('',#2794,#2773,#1554,.T.);
#3518=EDGE_CURVE('',#2795,#2785,#1555,.T.);
#3519=EDGE_CURVE('',#2791,#2795,#1556,.T.);
#3520=EDGE_CURVE('',#2794,#2790,#1557,.T.);
#3521=EDGE_CURVE('',#2795,#2796,#1558,.T.);
#3522=EDGE_CURVE('',#2796,#2797,#1559,.T.);
#3523=EDGE_CURVE('',#2798,#2797,#2278,.T.);
#3524=EDGE_CURVE('',#2798,#2799,#1560,.T.);
#3525=EDGE_CURVE('',#2800,#2799,#2279,.T.);
#3526=EDGE_CURVE('',#2801,#2800,#1561,.T.);
#3527=EDGE_CURVE('',#2801,#2802,#2280,.T.);
#3528=EDGE_CURVE('',#2803,#2802,#1562,.T.);
#3529=EDGE_CURVE('',#2804,#2803,#2281,.T.);
#3530=EDGE_CURVE('',#2789,#2804,#1563,.T.);
#3531=EDGE_CURVE('',#2805,#2805,#2282,.T.);
#3532=EDGE_CURVE('',#2796,#2784,#1564,.T.);
#3533=EDGE_CURVE('',#2797,#2783,#1565,.T.);
#3534=EDGE_CURVE('',#2805,#2772,#1566,.T.);
#3535=EDGE_CURVE('',#2798,#2782,#1567,.T.);
#3536=EDGE_CURVE('',#2799,#2781,#1568,.T.);
#3537=EDGE_CURVE('',#2800,#2780,#1569,.T.);
#3538=EDGE_CURVE('',#2801,#2779,#1570,.T.);
#3539=EDGE_CURVE('',#2802,#2778,#1571,.T.);
#3540=EDGE_CURVE('',#2803,#2777,#1572,.T.);
#3541=EDGE_CURVE('',#2804,#2776,#1573,.T.);
#3542=EDGE_CURVE('',#2806,#2806,#2283,.T.);
#3543=EDGE_CURVE('',#2806,#2807,#1574,.T.);
#3544=EDGE_CURVE('',#2807,#2807,#2284,.T.);
#3545=EDGE_CURVE('',#2808,#2808,#2285,.T.);
#3546=EDGE_CURVE('',#2808,#2809,#1575,.T.);
#3547=EDGE_CURVE('',#2809,#2809,#2286,.T.);
#3548=EDGE_CURVE('',#2810,#2811,#2287,.T.);
#3549=EDGE_CURVE('',#2811,#2810,#2288,.T.);
#3550=EDGE_CURVE('',#2811,#2812,#1576,.T.);
#3551=EDGE_CURVE('',#2812,#2812,#2289,.T.);
#3552=EDGE_CURVE('',#2810,#2813,#1577,.T.);
#3553=EDGE_CURVE('',#2813,#2813,#2290,.T.);
#3554=EDGE_CURVE('',#2814,#2814,#2291,.T.);
#3555=EDGE_CURVE('',#2814,#2815,#2292,.T.);
#3556=EDGE_CURVE('',#2815,#2815,#2293,.T.);
#3557=EDGE_CURVE('',#2816,#2816,#2294,.T.);
#3558=EDGE_CURVE('',#2816,#2814,#1578,.T.);
#3559=EDGE_CURVE('',#2817,#2817,#2295,.T.);
#3560=EDGE_CURVE('',#2817,#2816,#2296,.T.);
#3561=EDGE_CURVE('',#2807,#2818,#1579,.T.);
#3562=EDGE_CURVE('',#2818,#2818,#2297,.T.);
#3563=EDGE_CURVE('',#2819,#2820,#2298,.T.);
#3564=EDGE_CURVE('',#2820,#2821,#1580,.T.);
#3565=EDGE_CURVE('',#2821,#2821,#2299,.T.);
#3566=EDGE_CURVE('',#2820,#2819,#2300,.T.);
#3567=EDGE_CURVE('',#2819,#2822,#1581,.T.);
#3568=EDGE_CURVE('',#2822,#2822,#2301,.T.);
#3569=EDGE_CURVE('',#2822,#2823,#2302,.T.);
#3570=EDGE_CURVE('',#2823,#2823,#2303,.T.);
#3571=EDGE_CURVE('',#2824,#2824,#2304,.T.);
#3572=EDGE_CURVE('',#2824,#2825,#1582,.T.);
#3573=EDGE_CURVE('',#2825,#2825,#2305,.T.);
#3574=EDGE_CURVE('',#2826,#2826,#2306,.T.);
#3575=EDGE_CURVE('',#2826,#2827,#2307,.T.);
#3576=EDGE_CURVE('',#2827,#2827,#2308,.T.);
#3577=EDGE_CURVE('',#2827,#2828,#1583,.T.);
#3578=EDGE_CURVE('',#2828,#2828,#2309,.T.);
#3579=EDGE_CURVE('',#2828,#2829,#1584,.T.);
#3580=EDGE_CURVE('',#2829,#2829,#2310,.T.);
#3581=EDGE_CURVE('',#2830,#2830,#2311,.T.);
#3582=EDGE_CURVE('',#2830,#2831,#2312,.T.);
#3583=EDGE_CURVE('',#2831,#2831,#2313,.T.);
#3584=EDGE_CURVE('',#2831,#2832,#1585,.T.);
#3585=EDGE_CURVE('',#2832,#2832,#2314,.T.);
#3586=EDGE_CURVE('',#2832,#2833,#2315,.T.);
#3587=EDGE_CURVE('',#2833,#2833,#2316,.T.);
#3588=EDGE_CURVE('',#2834,#2834,#2317,.T.);
#3589=EDGE_CURVE('',#2834,#2835,#1586,.T.);
#3590=EDGE_CURVE('',#2835,#2835,#2318,.T.);
#3591=EDGE_CURVE('',#2836,#2836,#2319,.T.);
#3592=EDGE_CURVE('',#2836,#2837,#2320,.T.);
#3593=EDGE_CURVE('',#2837,#2837,#2321,.T.);
#3594=EDGE_CURVE('',#2838,#2838,#2322,.T.);
#3595=EDGE_CURVE('',#2838,#2836,#1587,.T.);
#3596=EDGE_CURVE('',#2839,#2839,#2323,.T.);
#3597=EDGE_CURVE('',#2839,#2838,#2324,.T.);
#3598=EDGE_CURVE('',#2840,#2840,#2325,.T.);
#3599=EDGE_CURVE('',#2840,#2841,#2326,.T.);
#3600=EDGE_CURVE('',#2841,#2841,#2327,.T.);
#3601=EDGE_CURVE('',#2842,#2842,#2328,.T.);
#3602=EDGE_CURVE('',#2842,#2840,#1588,.T.);
#3603=EDGE_CURVE('',#2843,#2843,#2329,.T.);
#3604=EDGE_CURVE('',#2843,#2842,#2330,.T.);
#3605=EDGE_CURVE('',#2844,#2844,#2331,.T.);
#3606=EDGE_CURVE('',#2844,#2845,#2332,.T.);
#3607=EDGE_CURVE('',#2845,#2845,#2333,.T.);
#3608=EDGE_CURVE('',#2846,#2846,#2334,.T.);
#3609=EDGE_CURVE('',#2846,#2844,#1589,.T.);
#3610=EDGE_CURVE('',#2847,#2847,#2335,.T.);
#3611=EDGE_CURVE('',#2847,#2846,#2336,.T.);
#3612=EDGE_CURVE('',#2848,#2848,#2337,.T.);
#3613=EDGE_CURVE('',#2848,#2849,#2338,.T.);
#3614=EDGE_CURVE('',#2849,#2849,#2339,.T.);
#3615=EDGE_CURVE('',#2850,#2850,#2340,.T.);
#3616=EDGE_CURVE('',#2850,#2848,#1590,.T.);
#3617=EDGE_CURVE('',#2851,#2851,#2341,.T.);
#3618=EDGE_CURVE('',#2851,#2852,#1591,.T.);
#3619=EDGE_CURVE('',#2852,#2852,#2342,.T.);
#3620=EDGE_CURVE('',#2853,#2853,#2343,.T.);
#3621=EDGE_CURVE('',#2853,#2854,#2344,.T.);
#3622=EDGE_CURVE('',#2854,#2854,#2345,.T.);
#3623=EDGE_CURVE('',#2855,#2855,#2346,.T.);
#3624=EDGE_CURVE('',#2855,#2853,#1592,.T.);
#3625=EDGE_CURVE('',#2856,#2856,#2347,.T.);
#3626=EDGE_CURVE('',#2856,#2855,#2348,.T.);
#3627=EDGE_CURVE('',#2857,#2857,#2349,.T.);
#3628=EDGE_CURVE('',#2857,#2858,#2350,.T.);
#3629=EDGE_CURVE('',#2858,#2858,#2351,.T.);
#3630=EDGE_CURVE('',#2859,#2859,#2352,.T.);
#3631=EDGE_CURVE('',#2859,#2857,#1593,.T.);
#3632=EDGE_CURVE('',#2860,#2860,#2353,.T.);
#3633=EDGE_CURVE('',#2860,#2859,#2354,.T.);
#3634=EDGE_CURVE('',#2861,#2861,#2355,.T.);
#3635=EDGE_CURVE('',#2861,#2862,#2356,.T.);
#3636=EDGE_CURVE('',#2862,#2862,#2357,.T.);
#3637=EDGE_CURVE('',#2863,#2863,#2358,.T.);
#3638=EDGE_CURVE('',#2863,#2861,#1594,.T.);
#3639=EDGE_CURVE('',#2864,#2864,#2359,.T.);
#3640=EDGE_CURVE('',#2864,#2863,#2360,.T.);
#3641=EDGE_CURVE('',#2865,#2865,#2361,.T.);
#3642=EDGE_CURVE('',#2865,#2866,#2362,.T.);
#3643=EDGE_CURVE('',#2866,#2866,#2363,.T.);
#3644=EDGE_CURVE('',#2867,#2867,#2364,.T.);
#3645=EDGE_CURVE('',#2867,#2865,#1595,.T.);
#3646=ORIENTED_EDGE('',*,*,#2868,.F.);
#3647=ORIENTED_EDGE('',*,*,#2869,.T.);
#3648=ORIENTED_EDGE('',*,*,#2870,.T.);
#3649=ORIENTED_EDGE('',*,*,#2869,.F.);
#3650=ORIENTED_EDGE('',*,*,#2871,.F.);
#3651=ORIENTED_EDGE('',*,*,#2872,.T.);
#3652=ORIENTED_EDGE('',*,*,#2873,.T.);
#3653=ORIENTED_EDGE('',*,*,#2872,.F.);
#3654=ORIENTED_EDGE('',*,*,#2874,.F.);
#3655=ORIENTED_EDGE('',*,*,#2875,.F.);
#3656=ORIENTED_EDGE('',*,*,#2876,.T.);
#3657=ORIENTED_EDGE('',*,*,#2877,.T.);
#3658=ORIENTED_EDGE('',*,*,#2876,.F.);
#3659=ORIENTED_EDGE('',*,*,#2874,.T.);
#3660=ORIENTED_EDGE('',*,*,#2875,.T.);
#3661=ORIENTED_EDGE('',*,*,#2878,.T.);
#3662=ORIENTED_EDGE('',*,*,#2879,.F.);
#3663=ORIENTED_EDGE('',*,*,#2878,.F.);
#3664=ORIENTED_EDGE('',*,*,#2880,.F.);
#3665=ORIENTED_EDGE('',*,*,#2881,.T.);
#3666=ORIENTED_EDGE('',*,*,#2882,.T.);
#3667=ORIENTED_EDGE('',*,*,#2881,.F.);
#3668=ORIENTED_EDGE('',*,*,#2883,.F.);
#3669=ORIENTED_EDGE('',*,*,#2884,.T.);
#3670=ORIENTED_EDGE('',*,*,#2880,.T.);
#3671=ORIENTED_EDGE('',*,*,#2884,.F.);
#3672=ORIENTED_EDGE('',*,*,#2885,.F.);
#3673=ORIENTED_EDGE('',*,*,#2886,.T.);
#3674=ORIENTED_EDGE('',*,*,#2883,.T.);
#3675=ORIENTED_EDGE('',*,*,#2886,.F.);
#3676=ORIENTED_EDGE('',*,*,#2870,.F.);
#3677=ORIENTED_EDGE('',*,*,#2887,.T.);
#3678=ORIENTED_EDGE('',*,*,#2888,.T.);
#3679=ORIENTED_EDGE('',*,*,#2887,.F.);
#3680=ORIENTED_EDGE('',*,*,#2885,.T.);
#3681=ORIENTED_EDGE('',*,*,#2888,.F.);
#3682=ORIENTED_EDGE('',*,*,#2882,.F.);
#3683=ORIENTED_EDGE('',*,*,#2879,.T.);
#3684=ORIENTED_EDGE('',*,*,#2871,.T.);
#3685=ORIENTED_EDGE('',*,*,#2877,.F.);
#3686=ORIENTED_EDGE('',*,*,#2873,.F.);
#3687=ORIENTED_EDGE('',*,*,#2868,.T.);
#3688=ORIENTED_EDGE('',*,*,#2889,.T.);
#3689=ORIENTED_EDGE('',*,*,#2890,.T.);
#3690=ORIENTED_EDGE('',*,*,#2891,.F.);
#3691=ORIENTED_EDGE('',*,*,#2890,.F.);
#3692=ORIENTED_EDGE('',*,*,#2892,.T.);
#3693=ORIENTED_EDGE('',*,*,#2889,.F.);
#3694=ORIENTED_EDGE('',*,*,#2893,.T.);
#3695=ORIENTED_EDGE('',*,*,#2894,.T.);
#3696=ORIENTED_EDGE('',*,*,#2893,.F.);
#3697=ORIENTED_EDGE('',*,*,#2892,.F.);
#3698=ORIENTED_EDGE('',*,*,#2894,.F.);
#3699=ORIENTED_EDGE('',*,*,#2895,.T.);
#3700=ORIENTED_EDGE('',*,*,#2896,.T.);
#3701=ORIENTED_EDGE('',*,*,#2895,.F.);
#3702=ORIENTED_EDGE('',*,*,#2897,.F.);
#3703=ORIENTED_EDGE('',*,*,#2898,.T.);
#3704=ORIENTED_EDGE('',*,*,#2899,.T.);
#3705=ORIENTED_EDGE('',*,*,#2898,.F.);
#3706=ORIENTED_EDGE('',*,*,#2900,.F.);
#3707=ORIENTED_EDGE('',*,*,#2901,.T.);
#3708=ORIENTED_EDGE('',*,*,#2902,.T.);
#3709=ORIENTED_EDGE('',*,*,#2901,.F.);
#3710=ORIENTED_EDGE('',*,*,#2902,.F.);
#3711=ORIENTED_EDGE('',*,*,#2903,.T.);
#3712=ORIENTED_EDGE('',*,*,#2904,.T.);
#3713=ORIENTED_EDGE('',*,*,#2903,.F.);
#3714=ORIENTED_EDGE('',*,*,#2904,.F.);
#3715=ORIENTED_EDGE('',*,*,#2905,.T.);
#3716=ORIENTED_EDGE('',*,*,#2906,.T.);
#3717=ORIENTED_EDGE('',*,*,#2905,.F.);
#3718=ORIENTED_EDGE('',*,*,#2907,.F.);
#3719=ORIENTED_EDGE('',*,*,#2908,.T.);
#3720=ORIENTED_EDGE('',*,*,#2909,.T.);
#3721=ORIENTED_EDGE('',*,*,#2908,.F.);
#3722=ORIENTED_EDGE('',*,*,#2909,.F.);
#3723=ORIENTED_EDGE('',*,*,#2910,.T.);
#3724=ORIENTED_EDGE('',*,*,#2911,.T.);
#3725=ORIENTED_EDGE('',*,*,#2910,.F.);
#3726=ORIENTED_EDGE('',*,*,#2911,.F.);
#3727=ORIENTED_EDGE('',*,*,#2912,.T.);
#3728=ORIENTED_EDGE('',*,*,#2913,.T.);
#3729=ORIENTED_EDGE('',*,*,#2912,.F.);
#3730=ORIENTED_EDGE('',*,*,#2906,.F.);
#3731=ORIENTED_EDGE('',*,*,#2907,.T.);
#3732=ORIENTED_EDGE('',*,*,#2899,.F.);
#3733=ORIENTED_EDGE('',*,*,#2900,.T.);
#3734=ORIENTED_EDGE('',*,*,#2897,.T.);
#3735=ORIENTED_EDGE('',*,*,#2896,.F.);
#3736=ORIENTED_EDGE('',*,*,#2891,.T.);
#3737=ORIENTED_EDGE('',*,*,#2913,.F.);
#3738=ORIENTED_EDGE('',*,*,#2914,.F.);
#3739=ORIENTED_EDGE('',*,*,#2915,.T.);
#3740=ORIENTED_EDGE('',*,*,#2916,.T.);
#3741=ORIENTED_EDGE('',*,*,#2915,.F.);
#3742=ORIENTED_EDGE('',*,*,#2917,.F.);
#3743=ORIENTED_EDGE('',*,*,#2918,.T.);
#3744=ORIENTED_EDGE('',*,*,#2919,.T.);
#3745=ORIENTED_EDGE('',*,*,#2918,.F.);
#3746=ORIENTED_EDGE('',*,*,#2920,.F.);
#3747=ORIENTED_EDGE('',*,*,#2921,.T.);
#3748=ORIENTED_EDGE('',*,*,#2917,.T.);
#3749=ORIENTED_EDGE('',*,*,#2921,.F.);
#3750=ORIENTED_EDGE('',*,*,#2922,.F.);
#3751=ORIENTED_EDGE('',*,*,#2923,.T.);
#3752=ORIENTED_EDGE('',*,*,#2920,.T.);
#3753=ORIENTED_EDGE('',*,*,#2923,.F.);
#3754=ORIENTED_EDGE('',*,*,#2924,.F.);
#3755=ORIENTED_EDGE('',*,*,#2925,.T.);
#3756=ORIENTED_EDGE('',*,*,#2926,.T.);
#3757=ORIENTED_EDGE('',*,*,#2925,.F.);
#3758=ORIENTED_EDGE('',*,*,#2927,.F.);
#3759=ORIENTED_EDGE('',*,*,#2928,.T.);
#3760=ORIENTED_EDGE('',*,*,#2924,.T.);
#3761=ORIENTED_EDGE('',*,*,#2928,.F.);
#3762=ORIENTED_EDGE('',*,*,#2929,.F.);
#3763=ORIENTED_EDGE('',*,*,#2930,.T.);
#3764=ORIENTED_EDGE('',*,*,#2927,.T.);
#3765=ORIENTED_EDGE('',*,*,#2930,.F.);
#3766=ORIENTED_EDGE('',*,*,#2931,.F.);
#3767=ORIENTED_EDGE('',*,*,#2932,.T.);
#3768=ORIENTED_EDGE('',*,*,#2933,.T.);
#3769=ORIENTED_EDGE('',*,*,#2932,.F.);
#3770=ORIENTED_EDGE('',*,*,#2934,.F.);
#3771=ORIENTED_EDGE('',*,*,#2935,.T.);
#3772=ORIENTED_EDGE('',*,*,#2931,.T.);
#3773=ORIENTED_EDGE('',*,*,#2935,.F.);
#3774=ORIENTED_EDGE('',*,*,#2936,.F.);
#3775=ORIENTED_EDGE('',*,*,#2937,.T.);
#3776=ORIENTED_EDGE('',*,*,#2934,.T.);
#3777=ORIENTED_EDGE('',*,*,#2937,.F.);
#3778=ORIENTED_EDGE('',*,*,#2938,.F.);
#3779=ORIENTED_EDGE('',*,*,#2939,.T.);
#3780=ORIENTED_EDGE('',*,*,#2940,.T.);
#3781=ORIENTED_EDGE('',*,*,#2939,.F.);
#3782=ORIENTED_EDGE('',*,*,#2941,.F.);
#3783=ORIENTED_EDGE('',*,*,#2942,.T.);
#3784=ORIENTED_EDGE('',*,*,#2938,.T.);
#3785=ORIENTED_EDGE('',*,*,#2942,.F.);
#3786=ORIENTED_EDGE('',*,*,#2941,.T.);
#3787=ORIENTED_EDGE('',*,*,#2916,.F.);
#3788=ORIENTED_EDGE('',*,*,#2936,.T.);
#3789=ORIENTED_EDGE('',*,*,#2940,.F.);
#3790=ORIENTED_EDGE('',*,*,#2929,.T.);
#3791=ORIENTED_EDGE('',*,*,#2933,.F.);
#3792=ORIENTED_EDGE('',*,*,#2926,.F.);
#3793=ORIENTED_EDGE('',*,*,#2922,.T.);
#3794=ORIENTED_EDGE('',*,*,#2919,.F.);
#3795=ORIENTED_EDGE('',*,*,#2914,.T.);
#3796=ORIENTED_EDGE('',*,*,#2943,.T.);
#3797=ORIENTED_EDGE('',*,*,#2944,.T.);
#3798=ORIENTED_EDGE('',*,*,#2945,.F.);
#3799=ORIENTED_EDGE('',*,*,#2944,.F.);
#3800=ORIENTED_EDGE('',*,*,#2946,.T.);
#3801=ORIENTED_EDGE('',*,*,#2947,.T.);
#3802=ORIENTED_EDGE('',*,*,#2948,.F.);
#3803=ORIENTED_EDGE('',*,*,#2947,.F.);
#3804=ORIENTED_EDGE('',*,*,#2949,.T.);
#3805=ORIENTED_EDGE('',*,*,#2950,.T.);
#3806=ORIENTED_EDGE('',*,*,#2946,.F.);
#3807=ORIENTED_EDGE('',*,*,#2950,.F.);
#3808=ORIENTED_EDGE('',*,*,#2951,.T.);
#3809=ORIENTED_EDGE('',*,*,#2952,.T.);
#3810=ORIENTED_EDGE('',*,*,#2949,.F.);
#3811=ORIENTED_EDGE('',*,*,#2952,.F.);
#3812=ORIENTED_EDGE('',*,*,#2953,.T.);
#3813=ORIENTED_EDGE('',*,*,#2954,.T.);
#3814=ORIENTED_EDGE('',*,*,#2955,.F.);
#3815=ORIENTED_EDGE('',*,*,#2954,.F.);
#3816=ORIENTED_EDGE('',*,*,#2956,.T.);
#3817=ORIENTED_EDGE('',*,*,#2957,.T.);
#3818=ORIENTED_EDGE('',*,*,#2953,.F.);
#3819=ORIENTED_EDGE('',*,*,#2957,.F.);
#3820=ORIENTED_EDGE('',*,*,#2958,.T.);
#3821=ORIENTED_EDGE('',*,*,#2959,.T.);
#3822=ORIENTED_EDGE('',*,*,#2956,.F.);
#3823=ORIENTED_EDGE('',*,*,#2959,.F.);
#3824=ORIENTED_EDGE('',*,*,#2960,.T.);
#3825=ORIENTED_EDGE('',*,*,#2961,.T.);
#3826=ORIENTED_EDGE('',*,*,#2962,.F.);
#3827=ORIENTED_EDGE('',*,*,#2961,.F.);
#3828=ORIENTED_EDGE('',*,*,#2963,.T.);
#3829=ORIENTED_EDGE('',*,*,#2964,.T.);
#3830=ORIENTED_EDGE('',*,*,#2960,.F.);
#3831=ORIENTED_EDGE('',*,*,#2964,.F.);
#3832=ORIENTED_EDGE('',*,*,#2965,.T.);
#3833=ORIENTED_EDGE('',*,*,#2966,.T.);
#3834=ORIENTED_EDGE('',*,*,#2963,.F.);
#3835=ORIENTED_EDGE('',*,*,#2966,.F.);
#3836=ORIENTED_EDGE('',*,*,#2967,.T.);
#3837=ORIENTED_EDGE('',*,*,#2968,.T.);
#3838=ORIENTED_EDGE('',*,*,#2969,.F.);
#3839=ORIENTED_EDGE('',*,*,#2968,.F.);
#3840=ORIENTED_EDGE('',*,*,#2970,.T.);
#3841=ORIENTED_EDGE('',*,*,#2971,.T.);
#3842=ORIENTED_EDGE('',*,*,#2967,.F.);
#3843=ORIENTED_EDGE('',*,*,#2971,.F.);
#3844=ORIENTED_EDGE('',*,*,#2970,.F.);
#3845=ORIENTED_EDGE('',*,*,#2945,.T.);
#3846=ORIENTED_EDGE('',*,*,#2965,.F.);
#3847=ORIENTED_EDGE('',*,*,#2969,.T.);
#3848=ORIENTED_EDGE('',*,*,#2958,.F.);
#3849=ORIENTED_EDGE('',*,*,#2962,.T.);
#3850=ORIENTED_EDGE('',*,*,#2955,.T.);
#3851=ORIENTED_EDGE('',*,*,#2951,.F.);
#3852=ORIENTED_EDGE('',*,*,#2948,.T.);
#3853=ORIENTED_EDGE('',*,*,#2943,.F.);
#3854=ORIENTED_EDGE('',*,*,#2972,.F.);
#3855=ORIENTED_EDGE('',*,*,#2973,.T.);
#3856=ORIENTED_EDGE('',*,*,#2974,.F.);
#3857=ORIENTED_EDGE('',*,*,#2973,.F.);
#3858=ORIENTED_EDGE('',*,*,#2975,.F.);
#3859=ORIENTED_EDGE('',*,*,#2976,.T.);
#3860=ORIENTED_EDGE('',*,*,#2977,.F.);
#3861=ORIENTED_EDGE('',*,*,#2978,.F.);
#3862=ORIENTED_EDGE('',*,*,#2979,.F.);
#3863=ORIENTED_EDGE('',*,*,#2980,.F.);
#3864=ORIENTED_EDGE('',*,*,#2981,.F.);
#3865=ORIENTED_EDGE('',*,*,#2982,.T.);
#3866=ORIENTED_EDGE('',*,*,#2983,.F.);
#3867=ORIENTED_EDGE('',*,*,#2982,.F.);
#3868=ORIENTED_EDGE('',*,*,#2984,.F.);
#3869=ORIENTED_EDGE('',*,*,#2985,.F.);
#3870=ORIENTED_EDGE('',*,*,#2976,.F.);
#3871=ORIENTED_EDGE('',*,*,#2980,.T.);
#3872=ORIENTED_EDGE('',*,*,#2986,.F.);
#3873=ORIENTED_EDGE('',*,*,#2978,.T.);
#3874=ORIENTED_EDGE('',*,*,#2987,.F.);
#3875=ORIENTED_EDGE('',*,*,#2988,.T.);
#3876=ORIENTED_EDGE('',*,*,#2989,.T.);
#3877=ORIENTED_EDGE('',*,*,#2984,.T.);
#3878=ORIENTED_EDGE('',*,*,#2981,.T.);
#3879=ORIENTED_EDGE('',*,*,#2986,.T.);
#3880=ORIENTED_EDGE('',*,*,#2979,.T.);
#3881=ORIENTED_EDGE('',*,*,#2983,.T.);
#3882=ORIENTED_EDGE('',*,*,#2975,.T.);
#3883=ORIENTED_EDGE('',*,*,#2987,.T.);
#3884=ORIENTED_EDGE('',*,*,#2977,.T.);
#3885=ORIENTED_EDGE('',*,*,#2985,.T.);
#3886=ORIENTED_EDGE('',*,*,#2989,.F.);
#3887=ORIENTED_EDGE('',*,*,#2990,.F.);
#3888=ORIENTED_EDGE('',*,*,#2991,.T.);
#3889=ORIENTED_EDGE('',*,*,#2988,.F.);
#3890=ORIENTED_EDGE('',*,*,#2991,.F.);
#3891=ORIENTED_EDGE('',*,*,#2974,.T.);
#3892=ORIENTED_EDGE('',*,*,#2990,.T.);
#3893=ORIENTED_EDGE('',*,*,#2992,.F.);
#3894=ORIENTED_EDGE('',*,*,#2993,.F.);
#3895=ORIENTED_EDGE('',*,*,#2994,.T.);
#3896=ORIENTED_EDGE('',*,*,#2992,.T.);
#3897=ORIENTED_EDGE('',*,*,#2994,.F.);
#3898=ORIENTED_EDGE('',*,*,#2995,.F.);
#3899=ORIENTED_EDGE('',*,*,#2996,.T.);
#3900=ORIENTED_EDGE('',*,*,#2993,.T.);
#3901=ORIENTED_EDGE('',*,*,#2996,.F.);
#3902=ORIENTED_EDGE('',*,*,#2972,.T.);
#3903=ORIENTED_EDGE('',*,*,#2997,.T.);
#3904=ORIENTED_EDGE('',*,*,#2995,.T.);
#3905=ORIENTED_EDGE('',*,*,#2997,.F.);
#3906=ORIENTED_EDGE('',*,*,#2998,.F.);
#3907=ORIENTED_EDGE('',*,*,#2999,.T.);
#3908=ORIENTED_EDGE('',*,*,#3000,.F.);
#3909=ORIENTED_EDGE('',*,*,#2999,.F.);
#3910=ORIENTED_EDGE('',*,*,#3001,.F.);
#3911=ORIENTED_EDGE('',*,*,#3002,.T.);
#3912=ORIENTED_EDGE('',*,*,#3003,.F.);
#3913=ORIENTED_EDGE('',*,*,#3002,.F.);
#3914=ORIENTED_EDGE('',*,*,#3004,.F.);
#3915=ORIENTED_EDGE('',*,*,#3005,.T.);
#3916=ORIENTED_EDGE('',*,*,#3006,.F.);
#3917=ORIENTED_EDGE('',*,*,#3005,.F.);
#3918=ORIENTED_EDGE('',*,*,#3007,.F.);
#3919=ORIENTED_EDGE('',*,*,#3008,.T.);
#3920=ORIENTED_EDGE('',*,*,#3009,.F.);
#3921=ORIENTED_EDGE('',*,*,#3008,.F.);
#3922=ORIENTED_EDGE('',*,*,#3007,.T.);
#3923=ORIENTED_EDGE('',*,*,#3006,.T.);
#3924=ORIENTED_EDGE('',*,*,#3010,.F.);
#3925=ORIENTED_EDGE('',*,*,#3011,.F.);
#3926=ORIENTED_EDGE('',*,*,#3012,.F.);
#3927=ORIENTED_EDGE('',*,*,#3013,.F.);
#3928=ORIENTED_EDGE('',*,*,#3014,.T.);
#3929=ORIENTED_EDGE('',*,*,#3009,.T.);
#3930=ORIENTED_EDGE('',*,*,#3015,.F.);
#3931=ORIENTED_EDGE('',*,*,#3016,.T.);
#3932=ORIENTED_EDGE('',*,*,#3017,.F.);
#3933=ORIENTED_EDGE('',*,*,#3016,.F.);
#3934=ORIENTED_EDGE('',*,*,#3018,.F.);
#3935=ORIENTED_EDGE('',*,*,#3019,.T.);
#3936=ORIENTED_EDGE('',*,*,#3014,.F.);
#3937=ORIENTED_EDGE('',*,*,#3019,.F.);
#3938=ORIENTED_EDGE('',*,*,#3018,.T.);
#3939=ORIENTED_EDGE('',*,*,#3017,.T.);
#3940=ORIENTED_EDGE('',*,*,#3004,.T.);
#3941=ORIENTED_EDGE('',*,*,#3001,.T.);
#3942=ORIENTED_EDGE('',*,*,#3011,.T.);
#3943=ORIENTED_EDGE('',*,*,#3020,.T.);
#3944=ORIENTED_EDGE('',*,*,#3021,.F.);
#3945=ORIENTED_EDGE('',*,*,#3022,.F.);
#3946=ORIENTED_EDGE('',*,*,#3012,.T.);
#3947=ORIENTED_EDGE('',*,*,#3022,.T.);
#3948=ORIENTED_EDGE('',*,*,#3023,.F.);
#3949=ORIENTED_EDGE('',*,*,#3024,.F.);
#3950=ORIENTED_EDGE('',*,*,#3013,.T.);
#3951=ORIENTED_EDGE('',*,*,#3024,.T.);
#3952=ORIENTED_EDGE('',*,*,#3025,.F.);
#3953=ORIENTED_EDGE('',*,*,#3026,.F.);
#3954=ORIENTED_EDGE('',*,*,#3010,.T.);
#3955=ORIENTED_EDGE('',*,*,#3026,.T.);
#3956=ORIENTED_EDGE('',*,*,#3027,.F.);
#3957=ORIENTED_EDGE('',*,*,#3020,.F.);
#3958=ORIENTED_EDGE('',*,*,#3027,.T.);
#3959=ORIENTED_EDGE('',*,*,#3025,.T.);
#3960=ORIENTED_EDGE('',*,*,#3023,.T.);
#3961=ORIENTED_EDGE('',*,*,#3021,.T.);
#3962=ORIENTED_EDGE('',*,*,#3000,.T.);
#3963=ORIENTED_EDGE('',*,*,#3003,.T.);
#3964=ORIENTED_EDGE('',*,*,#3015,.T.);
#3965=ORIENTED_EDGE('',*,*,#2998,.T.);
#3966=ORIENTED_EDGE('',*,*,#3028,.T.);
#3967=ORIENTED_EDGE('',*,*,#3029,.T.);
#3968=ORIENTED_EDGE('',*,*,#3030,.F.);
#3969=ORIENTED_EDGE('',*,*,#3029,.F.);
#3970=ORIENTED_EDGE('',*,*,#3031,.F.);
#3971=ORIENTED_EDGE('',*,*,#3032,.T.);
#3972=ORIENTED_EDGE('',*,*,#3033,.T.);
#3973=ORIENTED_EDGE('',*,*,#3032,.F.);
#3974=ORIENTED_EDGE('',*,*,#3031,.T.);
#3975=ORIENTED_EDGE('',*,*,#3030,.T.);
#3976=ORIENTED_EDGE('',*,*,#3033,.F.);
#3977=ORIENTED_EDGE('',*,*,#3028,.F.);
#3978=ORIENTED_EDGE('',*,*,#3034,.T.);
#3979=ORIENTED_EDGE('',*,*,#3035,.T.);
#3980=ORIENTED_EDGE('',*,*,#3036,.T.);
#3981=ORIENTED_EDGE('',*,*,#3037,.T.);
#3982=ORIENTED_EDGE('',*,*,#3035,.F.);
#3983=ORIENTED_EDGE('',*,*,#3037,.F.);
#3984=ORIENTED_EDGE('',*,*,#3038,.T.);
#3985=ORIENTED_EDGE('',*,*,#3039,.F.);
#3986=ORIENTED_EDGE('',*,*,#3040,.F.);
#3987=ORIENTED_EDGE('',*,*,#3038,.F.);
#3988=ORIENTED_EDGE('',*,*,#3036,.F.);
#3989=ORIENTED_EDGE('',*,*,#3034,.F.);
#3990=ORIENTED_EDGE('',*,*,#3041,.T.);
#3991=ORIENTED_EDGE('',*,*,#3042,.T.);
#3992=ORIENTED_EDGE('',*,*,#3043,.T.);
#3993=ORIENTED_EDGE('',*,*,#3044,.T.);
#3994=ORIENTED_EDGE('',*,*,#3042,.F.);
#3995=ORIENTED_EDGE('',*,*,#3045,.F.);
#3996=ORIENTED_EDGE('',*,*,#3046,.F.);
#3997=ORIENTED_EDGE('',*,*,#3047,.F.);
#3998=ORIENTED_EDGE('',*,*,#3048,.T.);
#3999=ORIENTED_EDGE('',*,*,#3043,.F.);
#4000=ORIENTED_EDGE('',*,*,#3044,.F.);
#4001=ORIENTED_EDGE('',*,*,#3048,.F.);
#4002=ORIENTED_EDGE('',*,*,#3041,.F.);
#4003=ORIENTED_EDGE('',*,*,#3049,.T.);
#4004=ORIENTED_EDGE('',*,*,#3050,.F.);
#4005=ORIENTED_EDGE('',*,*,#3051,.T.);
#4006=ORIENTED_EDGE('',*,*,#3047,.T.);
#4007=ORIENTED_EDGE('',*,*,#3052,.T.);
#4008=ORIENTED_EDGE('',*,*,#3049,.F.);
#4009=ORIENTED_EDGE('',*,*,#3052,.F.);
#4010=ORIENTED_EDGE('',*,*,#3046,.T.);
#4011=ORIENTED_EDGE('',*,*,#3045,.T.);
#4012=ORIENTED_EDGE('',*,*,#3051,.F.);
#4013=ORIENTED_EDGE('',*,*,#3039,.T.);
#4014=ORIENTED_EDGE('',*,*,#3040,.T.);
#4015=ORIENTED_EDGE('',*,*,#3050,.T.);
#4016=ORIENTED_EDGE('',*,*,#3053,.F.);
#4017=ORIENTED_EDGE('',*,*,#3054,.T.);
#4018=ORIENTED_EDGE('',*,*,#3055,.F.);
#4019=ORIENTED_EDGE('',*,*,#3056,.F.);
#4020=ORIENTED_EDGE('',*,*,#3057,.F.);
#4021=ORIENTED_EDGE('',*,*,#3056,.T.);
#4022=ORIENTED_EDGE('',*,*,#3058,.F.);
#4023=ORIENTED_EDGE('',*,*,#3059,.F.);
#4024=ORIENTED_EDGE('',*,*,#3060,.T.);
#4025=ORIENTED_EDGE('',*,*,#3061,.F.);
#4026=ORIENTED_EDGE('',*,*,#3062,.F.);
#4027=ORIENTED_EDGE('',*,*,#3054,.F.);
#4028=ORIENTED_EDGE('',*,*,#3059,.T.);
#4029=ORIENTED_EDGE('',*,*,#3063,.F.);
#4030=ORIENTED_EDGE('',*,*,#3064,.T.);
#4031=ORIENTED_EDGE('',*,*,#3065,.T.);
#4032=ORIENTED_EDGE('',*,*,#3061,.T.);
#4033=ORIENTED_EDGE('',*,*,#3066,.T.);
#4034=ORIENTED_EDGE('',*,*,#3067,.T.);
#4035=ORIENTED_EDGE('',*,*,#3068,.F.);
#4036=ORIENTED_EDGE('',*,*,#3069,.F.);
#4037=ORIENTED_EDGE('',*,*,#3070,.T.);
#4038=ORIENTED_EDGE('',*,*,#3071,.F.);
#4039=ORIENTED_EDGE('',*,*,#3072,.F.);
#4040=ORIENTED_EDGE('',*,*,#3073,.F.);
#4041=ORIENTED_EDGE('',*,*,#3072,.T.);
#4042=ORIENTED_EDGE('',*,*,#3074,.F.);
#4043=ORIENTED_EDGE('',*,*,#3075,.F.);
#4044=ORIENTED_EDGE('',*,*,#3076,.T.);
#4045=ORIENTED_EDGE('',*,*,#3064,.F.);
#4046=ORIENTED_EDGE('',*,*,#3077,.F.);
#4047=ORIENTED_EDGE('',*,*,#3070,.F.);
#4048=ORIENTED_EDGE('',*,*,#3075,.T.);
#4049=ORIENTED_EDGE('',*,*,#3078,.F.);
#4050=ORIENTED_EDGE('',*,*,#3079,.T.);
#4051=ORIENTED_EDGE('',*,*,#3080,.T.);
#4052=ORIENTED_EDGE('',*,*,#3081,.F.);
#4053=ORIENTED_EDGE('',*,*,#3082,.T.);
#4054=ORIENTED_EDGE('',*,*,#3083,.F.);
#4055=ORIENTED_EDGE('',*,*,#3084,.F.);
#4056=ORIENTED_EDGE('',*,*,#3085,.F.);
#4057=ORIENTED_EDGE('',*,*,#3084,.T.);
#4058=ORIENTED_EDGE('',*,*,#3086,.F.);
#4059=ORIENTED_EDGE('',*,*,#3087,.F.);
#4060=ORIENTED_EDGE('',*,*,#3088,.T.);
#4061=ORIENTED_EDGE('',*,*,#3079,.F.);
#4062=ORIENTED_EDGE('',*,*,#3089,.F.);
#4063=ORIENTED_EDGE('',*,*,#3082,.F.);
#4064=ORIENTED_EDGE('',*,*,#3087,.T.);
#4065=ORIENTED_EDGE('',*,*,#3090,.F.);
#4066=ORIENTED_EDGE('',*,*,#3091,.T.);
#4067=ORIENTED_EDGE('',*,*,#3092,.T.);
#4068=ORIENTED_EDGE('',*,*,#3093,.F.);
#4069=ORIENTED_EDGE('',*,*,#3094,.T.);
#4070=ORIENTED_EDGE('',*,*,#3095,.F.);
#4071=ORIENTED_EDGE('',*,*,#3096,.F.);
#4072=ORIENTED_EDGE('',*,*,#3097,.F.);
#4073=ORIENTED_EDGE('',*,*,#3096,.T.);
#4074=ORIENTED_EDGE('',*,*,#3098,.F.);
#4075=ORIENTED_EDGE('',*,*,#3099,.F.);
#4076=ORIENTED_EDGE('',*,*,#3100,.T.);
#4077=ORIENTED_EDGE('',*,*,#3091,.F.);
#4078=ORIENTED_EDGE('',*,*,#3101,.F.);
#4079=ORIENTED_EDGE('',*,*,#3094,.F.);
#4080=ORIENTED_EDGE('',*,*,#3099,.T.);
#4081=ORIENTED_EDGE('',*,*,#3102,.F.);
#4082=ORIENTED_EDGE('',*,*,#3103,.T.);
#4083=ORIENTED_EDGE('',*,*,#3104,.T.);
#4084=ORIENTED_EDGE('',*,*,#3105,.F.);
#4085=ORIENTED_EDGE('',*,*,#3106,.T.);
#4086=ORIENTED_EDGE('',*,*,#3107,.F.);
#4087=ORIENTED_EDGE('',*,*,#3108,.F.);
#4088=ORIENTED_EDGE('',*,*,#3109,.F.);
#4089=ORIENTED_EDGE('',*,*,#3108,.T.);
#4090=ORIENTED_EDGE('',*,*,#3110,.F.);
#4091=ORIENTED_EDGE('',*,*,#3111,.F.);
#4092=ORIENTED_EDGE('',*,*,#3112,.T.);
#4093=ORIENTED_EDGE('',*,*,#3103,.F.);
#4094=ORIENTED_EDGE('',*,*,#3113,.F.);
#4095=ORIENTED_EDGE('',*,*,#3106,.F.);
#4096=ORIENTED_EDGE('',*,*,#3111,.T.);
#4097=ORIENTED_EDGE('',*,*,#3114,.F.);
#4098=ORIENTED_EDGE('',*,*,#3115,.T.);
#4099=ORIENTED_EDGE('',*,*,#3116,.T.);
#4100=ORIENTED_EDGE('',*,*,#3117,.F.);
#4101=ORIENTED_EDGE('',*,*,#3118,.T.);
#4102=ORIENTED_EDGE('',*,*,#3119,.F.);
#4103=ORIENTED_EDGE('',*,*,#3120,.F.);
#4104=ORIENTED_EDGE('',*,*,#3121,.F.);
#4105=ORIENTED_EDGE('',*,*,#3120,.T.);
#4106=ORIENTED_EDGE('',*,*,#3122,.F.);
#4107=ORIENTED_EDGE('',*,*,#3123,.F.);
#4108=ORIENTED_EDGE('',*,*,#3124,.T.);
#4109=ORIENTED_EDGE('',*,*,#3125,.F.);
#4110=ORIENTED_EDGE('',*,*,#3126,.F.);
#4111=ORIENTED_EDGE('',*,*,#3118,.F.);
#4112=ORIENTED_EDGE('',*,*,#3123,.T.);
#4113=ORIENTED_EDGE('',*,*,#3127,.F.);
#4114=ORIENTED_EDGE('',*,*,#3128,.T.);
#4115=ORIENTED_EDGE('',*,*,#3129,.T.);
#4116=ORIENTED_EDGE('',*,*,#3125,.T.);
#4117=ORIENTED_EDGE('',*,*,#3130,.T.);
#4118=ORIENTED_EDGE('',*,*,#3131,.T.);
#4119=ORIENTED_EDGE('',*,*,#3132,.F.);
#4120=ORIENTED_EDGE('',*,*,#3133,.F.);
#4121=ORIENTED_EDGE('',*,*,#3134,.T.);
#4122=ORIENTED_EDGE('',*,*,#3135,.F.);
#4123=ORIENTED_EDGE('',*,*,#3136,.F.);
#4124=ORIENTED_EDGE('',*,*,#3137,.F.);
#4125=ORIENTED_EDGE('',*,*,#3136,.T.);
#4126=ORIENTED_EDGE('',*,*,#3138,.F.);
#4127=ORIENTED_EDGE('',*,*,#3131,.F.);
#4128=ORIENTED_EDGE('',*,*,#3139,.T.);
#4129=ORIENTED_EDGE('',*,*,#3115,.F.);
#4130=ORIENTED_EDGE('',*,*,#3140,.F.);
#4131=ORIENTED_EDGE('',*,*,#3134,.F.);
#4132=ORIENTED_EDGE('',*,*,#3141,.F.);
#4133=ORIENTED_EDGE('',*,*,#3142,.T.);
#4134=ORIENTED_EDGE('',*,*,#3143,.F.);
#4135=ORIENTED_EDGE('',*,*,#3144,.F.);
#4136=ORIENTED_EDGE('',*,*,#3145,.F.);
#4137=ORIENTED_EDGE('',*,*,#3144,.T.);
#4138=ORIENTED_EDGE('',*,*,#3146,.F.);
#4139=ORIENTED_EDGE('',*,*,#3147,.F.);
#4140=ORIENTED_EDGE('',*,*,#3148,.T.);
#4141=ORIENTED_EDGE('',*,*,#3128,.F.);
#4142=ORIENTED_EDGE('',*,*,#3149,.F.);
#4143=ORIENTED_EDGE('',*,*,#3142,.F.);
#4144=ORIENTED_EDGE('',*,*,#3147,.T.);
#4145=ORIENTED_EDGE('',*,*,#3150,.F.);
#4146=ORIENTED_EDGE('',*,*,#3151,.T.);
#4147=ORIENTED_EDGE('',*,*,#3152,.T.);
#4148=ORIENTED_EDGE('',*,*,#3153,.F.);
#4149=ORIENTED_EDGE('',*,*,#3154,.T.);
#4150=ORIENTED_EDGE('',*,*,#3155,.F.);
#4151=ORIENTED_EDGE('',*,*,#3156,.F.);
#4152=ORIENTED_EDGE('',*,*,#3157,.F.);
#4153=ORIENTED_EDGE('',*,*,#3156,.T.);
#4154=ORIENTED_EDGE('',*,*,#3158,.F.);
#4155=ORIENTED_EDGE('',*,*,#3159,.F.);
#4156=ORIENTED_EDGE('',*,*,#3160,.T.);
#4157=ORIENTED_EDGE('',*,*,#3161,.F.);
#4158=ORIENTED_EDGE('',*,*,#3162,.F.);
#4159=ORIENTED_EDGE('',*,*,#3154,.F.);
#4160=ORIENTED_EDGE('',*,*,#3159,.T.);
#4161=ORIENTED_EDGE('',*,*,#3163,.F.);
#4162=ORIENTED_EDGE('',*,*,#3164,.T.);
#4163=ORIENTED_EDGE('',*,*,#3165,.T.);
#4164=ORIENTED_EDGE('',*,*,#3161,.T.);
#4165=ORIENTED_EDGE('',*,*,#3166,.T.);
#4166=ORIENTED_EDGE('',*,*,#3167,.T.);
#4167=ORIENTED_EDGE('',*,*,#3168,.F.);
#4168=ORIENTED_EDGE('',*,*,#3169,.F.);
#4169=ORIENTED_EDGE('',*,*,#3170,.T.);
#4170=ORIENTED_EDGE('',*,*,#3171,.F.);
#4171=ORIENTED_EDGE('',*,*,#3172,.F.);
#4172=ORIENTED_EDGE('',*,*,#3173,.F.);
#4173=ORIENTED_EDGE('',*,*,#3172,.T.);
#4174=ORIENTED_EDGE('',*,*,#3174,.F.);
#4175=ORIENTED_EDGE('',*,*,#3175,.F.);
#4176=ORIENTED_EDGE('',*,*,#3176,.T.);
#4177=ORIENTED_EDGE('',*,*,#3177,.F.);
#4178=ORIENTED_EDGE('',*,*,#3178,.F.);
#4179=ORIENTED_EDGE('',*,*,#3170,.F.);
#4180=ORIENTED_EDGE('',*,*,#3175,.T.);
#4181=ORIENTED_EDGE('',*,*,#3179,.F.);
#4182=ORIENTED_EDGE('',*,*,#3180,.T.);
#4183=ORIENTED_EDGE('',*,*,#3181,.T.);
#4184=ORIENTED_EDGE('',*,*,#3177,.T.);
#4185=ORIENTED_EDGE('',*,*,#3182,.T.);
#4186=ORIENTED_EDGE('',*,*,#3183,.T.);
#4187=ORIENTED_EDGE('',*,*,#3184,.F.);
#4188=ORIENTED_EDGE('',*,*,#3185,.F.);
#4189=ORIENTED_EDGE('',*,*,#3186,.T.);
#4190=ORIENTED_EDGE('',*,*,#3187,.F.);
#4191=ORIENTED_EDGE('',*,*,#3188,.F.);
#4192=ORIENTED_EDGE('',*,*,#3189,.F.);
#4193=ORIENTED_EDGE('',*,*,#3188,.T.);
#4194=ORIENTED_EDGE('',*,*,#3190,.F.);
#4195=ORIENTED_EDGE('',*,*,#3183,.F.);
#4196=ORIENTED_EDGE('',*,*,#3191,.T.);
#4197=ORIENTED_EDGE('',*,*,#3164,.F.);
#4198=ORIENTED_EDGE('',*,*,#3192,.F.);
#4199=ORIENTED_EDGE('',*,*,#3186,.F.);
#4200=ORIENTED_EDGE('',*,*,#3193,.F.);
#4201=ORIENTED_EDGE('',*,*,#3194,.T.);
#4202=ORIENTED_EDGE('',*,*,#3195,.F.);
#4203=ORIENTED_EDGE('',*,*,#3196,.F.);
#4204=ORIENTED_EDGE('',*,*,#3197,.F.);
#4205=ORIENTED_EDGE('',*,*,#3196,.T.);
#4206=ORIENTED_EDGE('',*,*,#3198,.F.);
#4207=ORIENTED_EDGE('',*,*,#3167,.F.);
#4208=ORIENTED_EDGE('',*,*,#3199,.T.);
#4209=ORIENTED_EDGE('',*,*,#3151,.F.);
#4210=ORIENTED_EDGE('',*,*,#3200,.F.);
#4211=ORIENTED_EDGE('',*,*,#3194,.F.);
#4212=ORIENTED_EDGE('',*,*,#3201,.F.);
#4213=ORIENTED_EDGE('',*,*,#3202,.T.);
#4214=ORIENTED_EDGE('',*,*,#3203,.F.);
#4215=ORIENTED_EDGE('',*,*,#3204,.F.);
#4216=ORIENTED_EDGE('',*,*,#3205,.F.);
#4217=ORIENTED_EDGE('',*,*,#3204,.T.);
#4218=ORIENTED_EDGE('',*,*,#3206,.F.);
#4219=ORIENTED_EDGE('',*,*,#3207,.F.);
#4220=ORIENTED_EDGE('',*,*,#3208,.T.);
#4221=ORIENTED_EDGE('',*,*,#3180,.F.);
#4222=ORIENTED_EDGE('',*,*,#3209,.F.);
#4223=ORIENTED_EDGE('',*,*,#3202,.F.);
#4224=ORIENTED_EDGE('',*,*,#3207,.T.);
#4225=ORIENTED_EDGE('',*,*,#3210,.F.);
#4226=ORIENTED_EDGE('',*,*,#3211,.T.);
#4227=ORIENTED_EDGE('',*,*,#3212,.T.);
#4228=ORIENTED_EDGE('',*,*,#3213,.F.);
#4229=ORIENTED_EDGE('',*,*,#3214,.T.);
#4230=ORIENTED_EDGE('',*,*,#3215,.F.);
#4231=ORIENTED_EDGE('',*,*,#3216,.F.);
#4232=ORIENTED_EDGE('',*,*,#3217,.F.);
#4233=ORIENTED_EDGE('',*,*,#3216,.T.);
#4234=ORIENTED_EDGE('',*,*,#3218,.F.);
#4235=ORIENTED_EDGE('',*,*,#3219,.F.);
#4236=ORIENTED_EDGE('',*,*,#3220,.T.);
#4237=ORIENTED_EDGE('',*,*,#3211,.F.);
#4238=ORIENTED_EDGE('',*,*,#3221,.F.);
#4239=ORIENTED_EDGE('',*,*,#3214,.F.);
#4240=ORIENTED_EDGE('',*,*,#3219,.T.);
#4241=ORIENTED_EDGE('',*,*,#3222,.F.);
#4242=ORIENTED_EDGE('',*,*,#3223,.T.);
#4243=ORIENTED_EDGE('',*,*,#3224,.T.);
#4244=ORIENTED_EDGE('',*,*,#3225,.F.);
#4245=ORIENTED_EDGE('',*,*,#3226,.T.);
#4246=ORIENTED_EDGE('',*,*,#3227,.F.);
#4247=ORIENTED_EDGE('',*,*,#3228,.F.);
#4248=ORIENTED_EDGE('',*,*,#3229,.F.);
#4249=ORIENTED_EDGE('',*,*,#3228,.T.);
#4250=ORIENTED_EDGE('',*,*,#3230,.F.);
#4251=ORIENTED_EDGE('',*,*,#3231,.F.);
#4252=ORIENTED_EDGE('',*,*,#3232,.T.);
#4253=ORIENTED_EDGE('',*,*,#3233,.F.);
#4254=ORIENTED_EDGE('',*,*,#3234,.F.);
#4255=ORIENTED_EDGE('',*,*,#3226,.F.);
#4256=ORIENTED_EDGE('',*,*,#3231,.T.);
#4257=ORIENTED_EDGE('',*,*,#3235,.F.);
#4258=ORIENTED_EDGE('',*,*,#3236,.T.);
#4259=ORIENTED_EDGE('',*,*,#3237,.T.);
#4260=ORIENTED_EDGE('',*,*,#3233,.T.);
#4261=ORIENTED_EDGE('',*,*,#3238,.T.);
#4262=ORIENTED_EDGE('',*,*,#3239,.T.);
#4263=ORIENTED_EDGE('',*,*,#3240,.F.);
#4264=ORIENTED_EDGE('',*,*,#3241,.F.);
#4265=ORIENTED_EDGE('',*,*,#3242,.T.);
#4266=ORIENTED_EDGE('',*,*,#3243,.F.);
#4267=ORIENTED_EDGE('',*,*,#3244,.F.);
#4268=ORIENTED_EDGE('',*,*,#3245,.F.);
#4269=ORIENTED_EDGE('',*,*,#3244,.T.);
#4270=ORIENTED_EDGE('',*,*,#3246,.F.);
#4271=ORIENTED_EDGE('',*,*,#3247,.F.);
#4272=ORIENTED_EDGE('',*,*,#3248,.T.);
#4273=ORIENTED_EDGE('',*,*,#3223,.F.);
#4274=ORIENTED_EDGE('',*,*,#3249,.F.);
#4275=ORIENTED_EDGE('',*,*,#3242,.F.);
#4276=ORIENTED_EDGE('',*,*,#3247,.T.);
#4277=ORIENTED_EDGE('',*,*,#3250,.F.);
#4278=ORIENTED_EDGE('',*,*,#3251,.T.);
#4279=ORIENTED_EDGE('',*,*,#3252,.T.);
#4280=ORIENTED_EDGE('',*,*,#3253,.F.);
#4281=ORIENTED_EDGE('',*,*,#3254,.T.);
#4282=ORIENTED_EDGE('',*,*,#3255,.F.);
#4283=ORIENTED_EDGE('',*,*,#3256,.F.);
#4284=ORIENTED_EDGE('',*,*,#3257,.F.);
#4285=ORIENTED_EDGE('',*,*,#3256,.T.);
#4286=ORIENTED_EDGE('',*,*,#3258,.F.);
#4287=ORIENTED_EDGE('',*,*,#3259,.F.);
#4288=ORIENTED_EDGE('',*,*,#3260,.T.);
#4289=ORIENTED_EDGE('',*,*,#3251,.F.);
#4290=ORIENTED_EDGE('',*,*,#3261,.F.);
#4291=ORIENTED_EDGE('',*,*,#3254,.F.);
#4292=ORIENTED_EDGE('',*,*,#3259,.T.);
#4293=ORIENTED_EDGE('',*,*,#3262,.F.);
#4294=ORIENTED_EDGE('',*,*,#3263,.T.);
#4295=ORIENTED_EDGE('',*,*,#3264,.T.);
#4296=ORIENTED_EDGE('',*,*,#3265,.F.);
#4297=ORIENTED_EDGE('',*,*,#3266,.T.);
#4298=ORIENTED_EDGE('',*,*,#3267,.F.);
#4299=ORIENTED_EDGE('',*,*,#3268,.F.);
#4300=ORIENTED_EDGE('',*,*,#3269,.F.);
#4301=ORIENTED_EDGE('',*,*,#3268,.T.);
#4302=ORIENTED_EDGE('',*,*,#3270,.F.);
#4303=ORIENTED_EDGE('',*,*,#3239,.F.);
#4304=ORIENTED_EDGE('',*,*,#3271,.T.);
#4305=ORIENTED_EDGE('',*,*,#3263,.F.);
#4306=ORIENTED_EDGE('',*,*,#3272,.F.);
#4307=ORIENTED_EDGE('',*,*,#3266,.F.);
#4308=ORIENTED_EDGE('',*,*,#3273,.F.);
#4309=ORIENTED_EDGE('',*,*,#3274,.T.);
#4310=ORIENTED_EDGE('',*,*,#3275,.F.);
#4311=ORIENTED_EDGE('',*,*,#3276,.F.);
#4312=ORIENTED_EDGE('',*,*,#3277,.F.);
#4313=ORIENTED_EDGE('',*,*,#3276,.T.);
#4314=ORIENTED_EDGE('',*,*,#3278,.F.);
#4315=ORIENTED_EDGE('',*,*,#3279,.F.);
#4316=ORIENTED_EDGE('',*,*,#3280,.T.);
#4317=ORIENTED_EDGE('',*,*,#3281,.F.);
#4318=ORIENTED_EDGE('',*,*,#3282,.F.);
#4319=ORIENTED_EDGE('',*,*,#3274,.F.);
#4320=ORIENTED_EDGE('',*,*,#3279,.T.);
#4321=ORIENTED_EDGE('',*,*,#3283,.F.);
#4322=ORIENTED_EDGE('',*,*,#3284,.T.);
#4323=ORIENTED_EDGE('',*,*,#3285,.T.);
#4324=ORIENTED_EDGE('',*,*,#3281,.T.);
#4325=ORIENTED_EDGE('',*,*,#3286,.T.);
#4326=ORIENTED_EDGE('',*,*,#3287,.T.);
#4327=ORIENTED_EDGE('',*,*,#3288,.F.);
#4328=ORIENTED_EDGE('',*,*,#3289,.F.);
#4329=ORIENTED_EDGE('',*,*,#3290,.T.);
#4330=ORIENTED_EDGE('',*,*,#3291,.F.);
#4331=ORIENTED_EDGE('',*,*,#3292,.F.);
#4332=ORIENTED_EDGE('',*,*,#3293,.F.);
#4333=ORIENTED_EDGE('',*,*,#3292,.T.);
#4334=ORIENTED_EDGE('',*,*,#3294,.F.);
#4335=ORIENTED_EDGE('',*,*,#3287,.F.);
#4336=ORIENTED_EDGE('',*,*,#3295,.T.);
#4337=ORIENTED_EDGE('',*,*,#3236,.F.);
#4338=ORIENTED_EDGE('',*,*,#3296,.F.);
#4339=ORIENTED_EDGE('',*,*,#3290,.F.);
#4340=ORIENTED_EDGE('',*,*,#3297,.F.);
#4341=ORIENTED_EDGE('',*,*,#3298,.T.);
#4342=ORIENTED_EDGE('',*,*,#3299,.F.);
#4343=ORIENTED_EDGE('',*,*,#3300,.F.);
#4344=ORIENTED_EDGE('',*,*,#3301,.F.);
#4345=ORIENTED_EDGE('',*,*,#3300,.T.);
#4346=ORIENTED_EDGE('',*,*,#3302,.F.);
#4347=ORIENTED_EDGE('',*,*,#3303,.F.);
#4348=ORIENTED_EDGE('',*,*,#3304,.T.);
#4349=ORIENTED_EDGE('',*,*,#3305,.F.);
#4350=ORIENTED_EDGE('',*,*,#3306,.F.);
#4351=ORIENTED_EDGE('',*,*,#3298,.F.);
#4352=ORIENTED_EDGE('',*,*,#3303,.T.);
#4353=ORIENTED_EDGE('',*,*,#3307,.F.);
#4354=ORIENTED_EDGE('',*,*,#3308,.T.);
#4355=ORIENTED_EDGE('',*,*,#3309,.T.);
#4356=ORIENTED_EDGE('',*,*,#3305,.T.);
#4357=ORIENTED_EDGE('',*,*,#3310,.T.);
#4358=ORIENTED_EDGE('',*,*,#3311,.T.);
#4359=ORIENTED_EDGE('',*,*,#3312,.F.);
#4360=ORIENTED_EDGE('',*,*,#3313,.F.);
#4361=ORIENTED_EDGE('',*,*,#3314,.T.);
#4362=ORIENTED_EDGE('',*,*,#3315,.F.);
#4363=ORIENTED_EDGE('',*,*,#3316,.F.);
#4364=ORIENTED_EDGE('',*,*,#3317,.F.);
#4365=ORIENTED_EDGE('',*,*,#3316,.T.);
#4366=ORIENTED_EDGE('',*,*,#3318,.F.);
#4367=ORIENTED_EDGE('',*,*,#3067,.F.);
#4368=ORIENTED_EDGE('',*,*,#3319,.T.);
#4369=ORIENTED_EDGE('',*,*,#3308,.F.);
#4370=ORIENTED_EDGE('',*,*,#3320,.F.);
#4371=ORIENTED_EDGE('',*,*,#3314,.F.);
#4372=ORIENTED_EDGE('',*,*,#3321,.F.);
#4373=ORIENTED_EDGE('',*,*,#3322,.T.);
#4374=ORIENTED_EDGE('',*,*,#3323,.F.);
#4375=ORIENTED_EDGE('',*,*,#3324,.F.);
#4376=ORIENTED_EDGE('',*,*,#3325,.F.);
#4377=ORIENTED_EDGE('',*,*,#3324,.T.);
#4378=ORIENTED_EDGE('',*,*,#3326,.F.);
#4379=ORIENTED_EDGE('',*,*,#3327,.F.);
#4380=ORIENTED_EDGE('',*,*,#3328,.T.);
#4381=ORIENTED_EDGE('',*,*,#3329,.F.);
#4382=ORIENTED_EDGE('',*,*,#3330,.F.);
#4383=ORIENTED_EDGE('',*,*,#3322,.F.);
#4384=ORIENTED_EDGE('',*,*,#3327,.T.);
#4385=ORIENTED_EDGE('',*,*,#3331,.F.);
#4386=ORIENTED_EDGE('',*,*,#3332,.T.);
#4387=ORIENTED_EDGE('',*,*,#3333,.T.);
#4388=ORIENTED_EDGE('',*,*,#3329,.T.);
#4389=ORIENTED_EDGE('',*,*,#3334,.T.);
#4390=ORIENTED_EDGE('',*,*,#3335,.T.);
#4391=ORIENTED_EDGE('',*,*,#3336,.F.);
#4392=ORIENTED_EDGE('',*,*,#3337,.F.);
#4393=ORIENTED_EDGE('',*,*,#3338,.T.);
#4394=ORIENTED_EDGE('',*,*,#3339,.F.);
#4395=ORIENTED_EDGE('',*,*,#3340,.F.);
#4396=ORIENTED_EDGE('',*,*,#3341,.F.);
#4397=ORIENTED_EDGE('',*,*,#3340,.T.);
#4398=ORIENTED_EDGE('',*,*,#3342,.F.);
#4399=ORIENTED_EDGE('',*,*,#3343,.F.);
#4400=ORIENTED_EDGE('',*,*,#3344,.T.);
#4401=ORIENTED_EDGE('',*,*,#3332,.F.);
#4402=ORIENTED_EDGE('',*,*,#3345,.F.);
#4403=ORIENTED_EDGE('',*,*,#3338,.F.);
#4404=ORIENTED_EDGE('',*,*,#3343,.T.);
#4405=ORIENTED_EDGE('',*,*,#3346,.F.);
#4406=ORIENTED_EDGE('',*,*,#3347,.T.);
#4407=ORIENTED_EDGE('',*,*,#3348,.T.);
#4408=ORIENTED_EDGE('',*,*,#3349,.F.);
#4409=ORIENTED_EDGE('',*,*,#3350,.T.);
#4410=ORIENTED_EDGE('',*,*,#3351,.F.);
#4411=ORIENTED_EDGE('',*,*,#3352,.F.);
#4412=ORIENTED_EDGE('',*,*,#3353,.F.);
#4413=ORIENTED_EDGE('',*,*,#3352,.T.);
#4414=ORIENTED_EDGE('',*,*,#3354,.F.);
#4415=ORIENTED_EDGE('',*,*,#3355,.F.);
#4416=ORIENTED_EDGE('',*,*,#3356,.T.);
#4417=ORIENTED_EDGE('',*,*,#3347,.F.);
#4418=ORIENTED_EDGE('',*,*,#3357,.F.);
#4419=ORIENTED_EDGE('',*,*,#3350,.F.);
#4420=ORIENTED_EDGE('',*,*,#3355,.T.);
#4421=ORIENTED_EDGE('',*,*,#3358,.F.);
#4422=ORIENTED_EDGE('',*,*,#3359,.T.);
#4423=ORIENTED_EDGE('',*,*,#3360,.T.);
#4424=ORIENTED_EDGE('',*,*,#3361,.F.);
#4425=ORIENTED_EDGE('',*,*,#3362,.T.);
#4426=ORIENTED_EDGE('',*,*,#3363,.F.);
#4427=ORIENTED_EDGE('',*,*,#3364,.F.);
#4428=ORIENTED_EDGE('',*,*,#3365,.F.);
#4429=ORIENTED_EDGE('',*,*,#3364,.T.);
#4430=ORIENTED_EDGE('',*,*,#3366,.F.);
#4431=ORIENTED_EDGE('',*,*,#3335,.F.);
#4432=ORIENTED_EDGE('',*,*,#3367,.T.);
#4433=ORIENTED_EDGE('',*,*,#3368,.F.);
#4434=ORIENTED_EDGE('',*,*,#3369,.F.);
#4435=ORIENTED_EDGE('',*,*,#3362,.F.);
#4436=ORIENTED_EDGE('',*,*,#3368,.T.);
#4437=ORIENTED_EDGE('',*,*,#3370,.T.);
#4438=ORIENTED_EDGE('',*,*,#3371,.T.);
#4439=ORIENTED_EDGE('',*,*,#3372,.F.);
#4440=ORIENTED_EDGE('',*,*,#3373,.F.);
#4441=ORIENTED_EDGE('',*,*,#3374,.T.);
#4442=ORIENTED_EDGE('',*,*,#3375,.F.);
#4443=ORIENTED_EDGE('',*,*,#3376,.F.);
#4444=ORIENTED_EDGE('',*,*,#3377,.F.);
#4445=ORIENTED_EDGE('',*,*,#3376,.T.);
#4446=ORIENTED_EDGE('',*,*,#3378,.F.);
#4447=ORIENTED_EDGE('',*,*,#3379,.F.);
#4448=ORIENTED_EDGE('',*,*,#3380,.T.);
#4449=ORIENTED_EDGE('',*,*,#3381,.F.);
#4450=ORIENTED_EDGE('',*,*,#3382,.F.);
#4451=ORIENTED_EDGE('',*,*,#3374,.F.);
#4452=ORIENTED_EDGE('',*,*,#3379,.T.);
#4453=ORIENTED_EDGE('',*,*,#3383,.F.);
#4454=ORIENTED_EDGE('',*,*,#3384,.T.);
#4455=ORIENTED_EDGE('',*,*,#3385,.T.);
#4456=ORIENTED_EDGE('',*,*,#3381,.T.);
#4457=ORIENTED_EDGE('',*,*,#3386,.T.);
#4458=ORIENTED_EDGE('',*,*,#3387,.T.);
#4459=ORIENTED_EDGE('',*,*,#3388,.F.);
#4460=ORIENTED_EDGE('',*,*,#3389,.F.);
#4461=ORIENTED_EDGE('',*,*,#3390,.T.);
#4462=ORIENTED_EDGE('',*,*,#3391,.F.);
#4463=ORIENTED_EDGE('',*,*,#3392,.F.);
#4464=ORIENTED_EDGE('',*,*,#3393,.F.);
#4465=ORIENTED_EDGE('',*,*,#3392,.T.);
#4466=ORIENTED_EDGE('',*,*,#3394,.F.);
#4467=ORIENTED_EDGE('',*,*,#3371,.F.);
#4468=ORIENTED_EDGE('',*,*,#3395,.T.);
#4469=ORIENTED_EDGE('',*,*,#3384,.F.);
#4470=ORIENTED_EDGE('',*,*,#3396,.F.);
#4471=ORIENTED_EDGE('',*,*,#3390,.F.);
#4472=ORIENTED_EDGE('',*,*,#3397,.F.);
#4473=ORIENTED_EDGE('',*,*,#3398,.T.);
#4474=ORIENTED_EDGE('',*,*,#3399,.F.);
#4475=ORIENTED_EDGE('',*,*,#3400,.F.);
#4476=ORIENTED_EDGE('',*,*,#3401,.F.);
#4477=ORIENTED_EDGE('',*,*,#3400,.T.);
#4478=ORIENTED_EDGE('',*,*,#3402,.F.);
#4479=ORIENTED_EDGE('',*,*,#3387,.F.);
#4480=ORIENTED_EDGE('',*,*,#3403,.T.);
#4481=ORIENTED_EDGE('',*,*,#3284,.F.);
#4482=ORIENTED_EDGE('',*,*,#3404,.F.);
#4483=ORIENTED_EDGE('',*,*,#3398,.F.);
#4484=ORIENTED_EDGE('',*,*,#3405,.F.);
#4485=ORIENTED_EDGE('',*,*,#3406,.T.);
#4486=ORIENTED_EDGE('',*,*,#3407,.F.);
#4487=ORIENTED_EDGE('',*,*,#3408,.F.);
#4488=ORIENTED_EDGE('',*,*,#3409,.F.);
#4489=ORIENTED_EDGE('',*,*,#3408,.T.);
#4490=ORIENTED_EDGE('',*,*,#3410,.F.);
#4491=ORIENTED_EDGE('',*,*,#3311,.F.);
#4492=ORIENTED_EDGE('',*,*,#3411,.T.);
#4493=ORIENTED_EDGE('',*,*,#3359,.F.);
#4494=ORIENTED_EDGE('',*,*,#3412,.F.);
#4495=ORIENTED_EDGE('',*,*,#3406,.F.);
#4496=ORIENTED_EDGE('',*,*,#3413,.F.);
#4497=ORIENTED_EDGE('',*,*,#3414,.F.);
#4498=ORIENTED_EDGE('',*,*,#3415,.F.);
#4499=ORIENTED_EDGE('',*,*,#3416,.F.);
#4500=ORIENTED_EDGE('',*,*,#3417,.T.);
#4501=ORIENTED_EDGE('',*,*,#3418,.F.);
#4502=ORIENTED_EDGE('',*,*,#3419,.F.);
#4503=ORIENTED_EDGE('',*,*,#3420,.F.);
#4504=ORIENTED_EDGE('',*,*,#3416,.T.);
#4505=ORIENTED_EDGE('',*,*,#3421,.F.);
#4506=ORIENTED_EDGE('',*,*,#3422,.T.);
#4507=ORIENTED_EDGE('',*,*,#3423,.T.);
#4508=ORIENTED_EDGE('',*,*,#3418,.T.);
#4509=ORIENTED_EDGE('',*,*,#3424,.T.);
#4510=ORIENTED_EDGE('',*,*,#3425,.T.);
#4511=ORIENTED_EDGE('',*,*,#3426,.F.);
#4512=ORIENTED_EDGE('',*,*,#3420,.T.);
#4513=ORIENTED_EDGE('',*,*,#3427,.F.);
#4514=ORIENTED_EDGE('',*,*,#3428,.T.);
#4515=ORIENTED_EDGE('',*,*,#3429,.T.);
#4516=ORIENTED_EDGE('',*,*,#3414,.T.);
#4517=ORIENTED_EDGE('',*,*,#3430,.T.);
#4518=ORIENTED_EDGE('',*,*,#3431,.T.);
#4519=ORIENTED_EDGE('',*,*,#3432,.F.);
#4520=ORIENTED_EDGE('',*,*,#3433,.F.);
#4521=ORIENTED_EDGE('',*,*,#3428,.F.);
#4522=ORIENTED_EDGE('',*,*,#3434,.F.);
#4523=ORIENTED_EDGE('',*,*,#3425,.F.);
#4524=ORIENTED_EDGE('',*,*,#3435,.T.);
#4525=ORIENTED_EDGE('',*,*,#3436,.F.);
#4526=ORIENTED_EDGE('',*,*,#3437,.F.);
#4527=ORIENTED_EDGE('',*,*,#3438,.F.);
#4528=ORIENTED_EDGE('',*,*,#3436,.T.);
#4529=ORIENTED_EDGE('',*,*,#3439,.T.);
#4530=ORIENTED_EDGE('',*,*,#3440,.T.);
#4531=ORIENTED_EDGE('',*,*,#3441,.F.);
#4532=ORIENTED_EDGE('',*,*,#3438,.T.);
#4533=ORIENTED_EDGE('',*,*,#3442,.F.);
#4534=ORIENTED_EDGE('',*,*,#3443,.T.);
#4535=ORIENTED_EDGE('',*,*,#3444,.T.);
#4536=ORIENTED_EDGE('',*,*,#3445,.F.);
#4537=ORIENTED_EDGE('',*,*,#3443,.F.);
#4538=ORIENTED_EDGE('',*,*,#3446,.F.);
#4539=ORIENTED_EDGE('',*,*,#3440,.F.);
#4540=ORIENTED_EDGE('',*,*,#3447,.T.);
#4541=ORIENTED_EDGE('',*,*,#3448,.F.);
#4542=ORIENTED_EDGE('',*,*,#3449,.F.);
#4543=ORIENTED_EDGE('',*,*,#3450,.F.);
#4544=ORIENTED_EDGE('',*,*,#3448,.T.);
#4545=ORIENTED_EDGE('',*,*,#3451,.T.);
#4546=ORIENTED_EDGE('',*,*,#3452,.T.);
#4547=ORIENTED_EDGE('',*,*,#3453,.F.);
#4548=ORIENTED_EDGE('',*,*,#3450,.T.);
#4549=ORIENTED_EDGE('',*,*,#3454,.F.);
#4550=ORIENTED_EDGE('',*,*,#3455,.T.);
#4551=ORIENTED_EDGE('',*,*,#3456,.T.);
#4552=ORIENTED_EDGE('',*,*,#3457,.F.);
#4553=ORIENTED_EDGE('',*,*,#3455,.F.);
#4554=ORIENTED_EDGE('',*,*,#3458,.F.);
#4555=ORIENTED_EDGE('',*,*,#3452,.F.);
#4556=ORIENTED_EDGE('',*,*,#3459,.T.);
#4557=ORIENTED_EDGE('',*,*,#3460,.F.);
#4558=ORIENTED_EDGE('',*,*,#3461,.F.);
#4559=ORIENTED_EDGE('',*,*,#3462,.F.);
#4560=ORIENTED_EDGE('',*,*,#3460,.T.);
#4561=ORIENTED_EDGE('',*,*,#3463,.T.);
#4562=ORIENTED_EDGE('',*,*,#3464,.T.);
#4563=ORIENTED_EDGE('',*,*,#3465,.F.);
#4564=ORIENTED_EDGE('',*,*,#3462,.T.);
#4565=ORIENTED_EDGE('',*,*,#3466,.F.);
#4566=ORIENTED_EDGE('',*,*,#3467,.T.);
#4567=ORIENTED_EDGE('',*,*,#3468,.T.);
#4568=ORIENTED_EDGE('',*,*,#3469,.F.);
#4569=ORIENTED_EDGE('',*,*,#3467,.F.);
#4570=ORIENTED_EDGE('',*,*,#3470,.F.);
#4571=ORIENTED_EDGE('',*,*,#3464,.F.);
#4572=ORIENTED_EDGE('',*,*,#3471,.T.);
#4573=ORIENTED_EDGE('',*,*,#3472,.F.);
#4574=ORIENTED_EDGE('',*,*,#3473,.F.);
#4575=ORIENTED_EDGE('',*,*,#3474,.F.);
#4576=ORIENTED_EDGE('',*,*,#3472,.T.);
#4577=ORIENTED_EDGE('',*,*,#3475,.T.);
#4578=ORIENTED_EDGE('',*,*,#3476,.T.);
#4579=ORIENTED_EDGE('',*,*,#3477,.F.);
#4580=ORIENTED_EDGE('',*,*,#3474,.T.);
#4581=ORIENTED_EDGE('',*,*,#3478,.F.);
#4582=ORIENTED_EDGE('',*,*,#3479,.T.);
#4583=ORIENTED_EDGE('',*,*,#3480,.T.);
#4584=ORIENTED_EDGE('',*,*,#3481,.F.);
#4585=ORIENTED_EDGE('',*,*,#3479,.F.);
#4586=ORIENTED_EDGE('',*,*,#3482,.F.);
#4587=ORIENTED_EDGE('',*,*,#3476,.F.);
#4588=ORIENTED_EDGE('',*,*,#3483,.T.);
#4589=ORIENTED_EDGE('',*,*,#3422,.F.);
#4590=ORIENTED_EDGE('',*,*,#3484,.F.);
#4591=ORIENTED_EDGE('',*,*,#3431,.F.);
#4592=ORIENTED_EDGE('',*,*,#3485,.T.);
#4593=ORIENTED_EDGE('',*,*,#3486,.T.);
#4594=ORIENTED_EDGE('',*,*,#3487,.F.);
#4595=ORIENTED_EDGE('',*,*,#3486,.F.);
#4596=ORIENTED_EDGE('',*,*,#3358,.T.);
#4597=ORIENTED_EDGE('',*,*,#3354,.T.);
#4598=ORIENTED_EDGE('',*,*,#3351,.T.);
#4599=ORIENTED_EDGE('',*,*,#3357,.T.);
#4600=ORIENTED_EDGE('',*,*,#3346,.T.);
#4601=ORIENTED_EDGE('',*,*,#3342,.T.);
#4602=ORIENTED_EDGE('',*,*,#3339,.T.);
#4603=ORIENTED_EDGE('',*,*,#3345,.T.);
#4604=ORIENTED_EDGE('',*,*,#3331,.T.);
#4605=ORIENTED_EDGE('',*,*,#3326,.T.);
#4606=ORIENTED_EDGE('',*,*,#3323,.T.);
#4607=ORIENTED_EDGE('',*,*,#3330,.T.);
#4608=ORIENTED_EDGE('',*,*,#3336,.T.);
#4609=ORIENTED_EDGE('',*,*,#3366,.T.);
#4610=ORIENTED_EDGE('',*,*,#3363,.T.);
#4611=ORIENTED_EDGE('',*,*,#3369,.T.);
#4612=ORIENTED_EDGE('',*,*,#3372,.T.);
#4613=ORIENTED_EDGE('',*,*,#3394,.T.);
#4614=ORIENTED_EDGE('',*,*,#3391,.T.);
#4615=ORIENTED_EDGE('',*,*,#3396,.T.);
#4616=ORIENTED_EDGE('',*,*,#3383,.T.);
#4617=ORIENTED_EDGE('',*,*,#3378,.T.);
#4618=ORIENTED_EDGE('',*,*,#3375,.T.);
#4619=ORIENTED_EDGE('',*,*,#3382,.T.);
#4620=ORIENTED_EDGE('',*,*,#3388,.T.);
#4621=ORIENTED_EDGE('',*,*,#3402,.T.);
#4622=ORIENTED_EDGE('',*,*,#3399,.T.);
#4623=ORIENTED_EDGE('',*,*,#3404,.T.);
#4624=ORIENTED_EDGE('',*,*,#3283,.T.);
#4625=ORIENTED_EDGE('',*,*,#3278,.T.);
#4626=ORIENTED_EDGE('',*,*,#3275,.T.);
#4627=ORIENTED_EDGE('',*,*,#3282,.T.);
#4628=ORIENTED_EDGE('',*,*,#3288,.T.);
#4629=ORIENTED_EDGE('',*,*,#3294,.T.);
#4630=ORIENTED_EDGE('',*,*,#3291,.T.);
#4631=ORIENTED_EDGE('',*,*,#3296,.T.);
#4632=ORIENTED_EDGE('',*,*,#3235,.T.);
#4633=ORIENTED_EDGE('',*,*,#3230,.T.);
#4634=ORIENTED_EDGE('',*,*,#3227,.T.);
#4635=ORIENTED_EDGE('',*,*,#3234,.T.);
#4636=ORIENTED_EDGE('',*,*,#3240,.T.);
#4637=ORIENTED_EDGE('',*,*,#3270,.T.);
#4638=ORIENTED_EDGE('',*,*,#3267,.T.);
#4639=ORIENTED_EDGE('',*,*,#3272,.T.);
#4640=ORIENTED_EDGE('',*,*,#3262,.T.);
#4641=ORIENTED_EDGE('',*,*,#3258,.T.);
#4642=ORIENTED_EDGE('',*,*,#3255,.T.);
#4643=ORIENTED_EDGE('',*,*,#3261,.T.);
#4644=ORIENTED_EDGE('',*,*,#3250,.T.);
#4645=ORIENTED_EDGE('',*,*,#3246,.T.);
#4646=ORIENTED_EDGE('',*,*,#3243,.T.);
#4647=ORIENTED_EDGE('',*,*,#3249,.T.);
#4648=ORIENTED_EDGE('',*,*,#3222,.T.);
#4649=ORIENTED_EDGE('',*,*,#3218,.T.);
#4650=ORIENTED_EDGE('',*,*,#3215,.T.);
#4651=ORIENTED_EDGE('',*,*,#3221,.T.);
#4652=ORIENTED_EDGE('',*,*,#3210,.T.);
#4653=ORIENTED_EDGE('',*,*,#3206,.T.);
#4654=ORIENTED_EDGE('',*,*,#3203,.T.);
#4655=ORIENTED_EDGE('',*,*,#3209,.T.);
#4656=ORIENTED_EDGE('',*,*,#3179,.T.);
#4657=ORIENTED_EDGE('',*,*,#3174,.T.);
#4658=ORIENTED_EDGE('',*,*,#3171,.T.);
#4659=ORIENTED_EDGE('',*,*,#3178,.T.);
#4660=ORIENTED_EDGE('',*,*,#3184,.T.);
#4661=ORIENTED_EDGE('',*,*,#3190,.T.);
#4662=ORIENTED_EDGE('',*,*,#3187,.T.);
#4663=ORIENTED_EDGE('',*,*,#3192,.T.);
#4664=ORIENTED_EDGE('',*,*,#3163,.T.);
#4665=ORIENTED_EDGE('',*,*,#3158,.T.);
#4666=ORIENTED_EDGE('',*,*,#3155,.T.);
#4667=ORIENTED_EDGE('',*,*,#3162,.T.);
#4668=ORIENTED_EDGE('',*,*,#3168,.T.);
#4669=ORIENTED_EDGE('',*,*,#3198,.T.);
#4670=ORIENTED_EDGE('',*,*,#3195,.T.);
#4671=ORIENTED_EDGE('',*,*,#3200,.T.);
#4672=ORIENTED_EDGE('',*,*,#3150,.T.);
#4673=ORIENTED_EDGE('',*,*,#3146,.T.);
#4674=ORIENTED_EDGE('',*,*,#3143,.T.);
#4675=ORIENTED_EDGE('',*,*,#3149,.T.);
#4676=ORIENTED_EDGE('',*,*,#3127,.T.);
#4677=ORIENTED_EDGE('',*,*,#3122,.T.);
#4678=ORIENTED_EDGE('',*,*,#3119,.T.);
#4679=ORIENTED_EDGE('',*,*,#3126,.T.);
#4680=ORIENTED_EDGE('',*,*,#3132,.T.);
#4681=ORIENTED_EDGE('',*,*,#3138,.T.);
#4682=ORIENTED_EDGE('',*,*,#3135,.T.);
#4683=ORIENTED_EDGE('',*,*,#3140,.T.);
#4684=ORIENTED_EDGE('',*,*,#3114,.T.);
#4685=ORIENTED_EDGE('',*,*,#3110,.T.);
#4686=ORIENTED_EDGE('',*,*,#3107,.T.);
#4687=ORIENTED_EDGE('',*,*,#3113,.T.);
#4688=ORIENTED_EDGE('',*,*,#3102,.T.);
#4689=ORIENTED_EDGE('',*,*,#3098,.T.);
#4690=ORIENTED_EDGE('',*,*,#3095,.T.);
#4691=ORIENTED_EDGE('',*,*,#3101,.T.);
#4692=ORIENTED_EDGE('',*,*,#3090,.T.);
#4693=ORIENTED_EDGE('',*,*,#3086,.T.);
#4694=ORIENTED_EDGE('',*,*,#3083,.T.);
#4695=ORIENTED_EDGE('',*,*,#3089,.T.);
#4696=ORIENTED_EDGE('',*,*,#3078,.T.);
#4697=ORIENTED_EDGE('',*,*,#3074,.T.);
#4698=ORIENTED_EDGE('',*,*,#3071,.T.);
#4699=ORIENTED_EDGE('',*,*,#3077,.T.);
#4700=ORIENTED_EDGE('',*,*,#3063,.T.);
#4701=ORIENTED_EDGE('',*,*,#3058,.T.);
#4702=ORIENTED_EDGE('',*,*,#3055,.T.);
#4703=ORIENTED_EDGE('',*,*,#3062,.T.);
#4704=ORIENTED_EDGE('',*,*,#3068,.T.);
#4705=ORIENTED_EDGE('',*,*,#3318,.T.);
#4706=ORIENTED_EDGE('',*,*,#3315,.T.);
#4707=ORIENTED_EDGE('',*,*,#3320,.T.);
#4708=ORIENTED_EDGE('',*,*,#3307,.T.);
#4709=ORIENTED_EDGE('',*,*,#3302,.T.);
#4710=ORIENTED_EDGE('',*,*,#3299,.T.);
#4711=ORIENTED_EDGE('',*,*,#3306,.T.);
#4712=ORIENTED_EDGE('',*,*,#3312,.T.);
#4713=ORIENTED_EDGE('',*,*,#3410,.T.);
#4714=ORIENTED_EDGE('',*,*,#3407,.T.);
#4715=ORIENTED_EDGE('',*,*,#3412,.T.);
#4716=ORIENTED_EDGE('',*,*,#3426,.T.);
#4717=ORIENTED_EDGE('',*,*,#3434,.T.);
#4718=ORIENTED_EDGE('',*,*,#3427,.T.);
#4719=ORIENTED_EDGE('',*,*,#3419,.T.);
#4720=ORIENTED_EDGE('',*,*,#3441,.T.);
#4721=ORIENTED_EDGE('',*,*,#3446,.T.);
#4722=ORIENTED_EDGE('',*,*,#3442,.T.);
#4723=ORIENTED_EDGE('',*,*,#3437,.T.);
#4724=ORIENTED_EDGE('',*,*,#3453,.T.);
#4725=ORIENTED_EDGE('',*,*,#3458,.T.);
#4726=ORIENTED_EDGE('',*,*,#3454,.T.);
#4727=ORIENTED_EDGE('',*,*,#3449,.T.);
#4728=ORIENTED_EDGE('',*,*,#3465,.T.);
#4729=ORIENTED_EDGE('',*,*,#3470,.T.);
#4730=ORIENTED_EDGE('',*,*,#3466,.T.);
#4731=ORIENTED_EDGE('',*,*,#3461,.T.);
#4732=ORIENTED_EDGE('',*,*,#3477,.T.);
#4733=ORIENTED_EDGE('',*,*,#3482,.T.);
#4734=ORIENTED_EDGE('',*,*,#3478,.T.);
#4735=ORIENTED_EDGE('',*,*,#3473,.T.);
#4736=ORIENTED_EDGE('',*,*,#3487,.T.);
#4737=ORIENTED_EDGE('',*,*,#3415,.T.);
#4738=ORIENTED_EDGE('',*,*,#3432,.T.);
#4739=ORIENTED_EDGE('',*,*,#3484,.T.);
#4740=ORIENTED_EDGE('',*,*,#3421,.T.);
#4741=ORIENTED_EDGE('',*,*,#3360,.F.);
#4742=ORIENTED_EDGE('',*,*,#3411,.F.);
#4743=ORIENTED_EDGE('',*,*,#3405,.T.);
#4744=ORIENTED_EDGE('',*,*,#3409,.T.);
#4745=ORIENTED_EDGE('',*,*,#3310,.F.);
#4746=ORIENTED_EDGE('',*,*,#3304,.F.);
#4747=ORIENTED_EDGE('',*,*,#3297,.T.);
#4748=ORIENTED_EDGE('',*,*,#3301,.T.);
#4749=ORIENTED_EDGE('',*,*,#3309,.F.);
#4750=ORIENTED_EDGE('',*,*,#3319,.F.);
#4751=ORIENTED_EDGE('',*,*,#3313,.T.);
#4752=ORIENTED_EDGE('',*,*,#3317,.T.);
#4753=ORIENTED_EDGE('',*,*,#3066,.F.);
#4754=ORIENTED_EDGE('',*,*,#3060,.F.);
#4755=ORIENTED_EDGE('',*,*,#3053,.T.);
#4756=ORIENTED_EDGE('',*,*,#3057,.T.);
#4757=ORIENTED_EDGE('',*,*,#3065,.F.);
#4758=ORIENTED_EDGE('',*,*,#3076,.F.);
#4759=ORIENTED_EDGE('',*,*,#3069,.T.);
#4760=ORIENTED_EDGE('',*,*,#3073,.T.);
#4761=ORIENTED_EDGE('',*,*,#3080,.F.);
#4762=ORIENTED_EDGE('',*,*,#3088,.F.);
#4763=ORIENTED_EDGE('',*,*,#3081,.T.);
#4764=ORIENTED_EDGE('',*,*,#3085,.T.);
#4765=ORIENTED_EDGE('',*,*,#3092,.F.);
#4766=ORIENTED_EDGE('',*,*,#3100,.F.);
#4767=ORIENTED_EDGE('',*,*,#3093,.T.);
#4768=ORIENTED_EDGE('',*,*,#3097,.T.);
#4769=ORIENTED_EDGE('',*,*,#3104,.F.);
#4770=ORIENTED_EDGE('',*,*,#3112,.F.);
#4771=ORIENTED_EDGE('',*,*,#3105,.T.);
#4772=ORIENTED_EDGE('',*,*,#3109,.T.);
#4773=ORIENTED_EDGE('',*,*,#3116,.F.);
#4774=ORIENTED_EDGE('',*,*,#3139,.F.);
#4775=ORIENTED_EDGE('',*,*,#3133,.T.);
#4776=ORIENTED_EDGE('',*,*,#3137,.T.);
#4777=ORIENTED_EDGE('',*,*,#3130,.F.);
#4778=ORIENTED_EDGE('',*,*,#3124,.F.);
#4779=ORIENTED_EDGE('',*,*,#3117,.T.);
#4780=ORIENTED_EDGE('',*,*,#3121,.T.);
#4781=ORIENTED_EDGE('',*,*,#3129,.F.);
#4782=ORIENTED_EDGE('',*,*,#3148,.F.);
#4783=ORIENTED_EDGE('',*,*,#3141,.T.);
#4784=ORIENTED_EDGE('',*,*,#3145,.T.);
#4785=ORIENTED_EDGE('',*,*,#3152,.F.);
#4786=ORIENTED_EDGE('',*,*,#3199,.F.);
#4787=ORIENTED_EDGE('',*,*,#3193,.T.);
#4788=ORIENTED_EDGE('',*,*,#3197,.T.);
#4789=ORIENTED_EDGE('',*,*,#3166,.F.);
#4790=ORIENTED_EDGE('',*,*,#3160,.F.);
#4791=ORIENTED_EDGE('',*,*,#3153,.T.);
#4792=ORIENTED_EDGE('',*,*,#3157,.T.);
#4793=ORIENTED_EDGE('',*,*,#3165,.F.);
#4794=ORIENTED_EDGE('',*,*,#3191,.F.);
#4795=ORIENTED_EDGE('',*,*,#3185,.T.);
#4796=ORIENTED_EDGE('',*,*,#3189,.T.);
#4797=ORIENTED_EDGE('',*,*,#3182,.F.);
#4798=ORIENTED_EDGE('',*,*,#3176,.F.);
#4799=ORIENTED_EDGE('',*,*,#3169,.T.);
#4800=ORIENTED_EDGE('',*,*,#3173,.T.);
#4801=ORIENTED_EDGE('',*,*,#3181,.F.);
#4802=ORIENTED_EDGE('',*,*,#3208,.F.);
#4803=ORIENTED_EDGE('',*,*,#3201,.T.);
#4804=ORIENTED_EDGE('',*,*,#3205,.T.);
#4805=ORIENTED_EDGE('',*,*,#3212,.F.);
#4806=ORIENTED_EDGE('',*,*,#3220,.F.);
#4807=ORIENTED_EDGE('',*,*,#3213,.T.);
#4808=ORIENTED_EDGE('',*,*,#3217,.T.);
#4809=ORIENTED_EDGE('',*,*,#3224,.F.);
#4810=ORIENTED_EDGE('',*,*,#3248,.F.);
#4811=ORIENTED_EDGE('',*,*,#3241,.T.);
#4812=ORIENTED_EDGE('',*,*,#3245,.T.);
#4813=ORIENTED_EDGE('',*,*,#3252,.F.);
#4814=ORIENTED_EDGE('',*,*,#3260,.F.);
#4815=ORIENTED_EDGE('',*,*,#3253,.T.);
#4816=ORIENTED_EDGE('',*,*,#3257,.T.);
#4817=ORIENTED_EDGE('',*,*,#3264,.F.);
#4818=ORIENTED_EDGE('',*,*,#3271,.F.);
#4819=ORIENTED_EDGE('',*,*,#3265,.T.);
#4820=ORIENTED_EDGE('',*,*,#3269,.T.);
#4821=ORIENTED_EDGE('',*,*,#3238,.F.);
#4822=ORIENTED_EDGE('',*,*,#3232,.F.);
#4823=ORIENTED_EDGE('',*,*,#3225,.T.);
#4824=ORIENTED_EDGE('',*,*,#3229,.T.);
#4825=ORIENTED_EDGE('',*,*,#3237,.F.);
#4826=ORIENTED_EDGE('',*,*,#3295,.F.);
#4827=ORIENTED_EDGE('',*,*,#3289,.T.);
#4828=ORIENTED_EDGE('',*,*,#3293,.T.);
#4829=ORIENTED_EDGE('',*,*,#3286,.F.);
#4830=ORIENTED_EDGE('',*,*,#3280,.F.);
#4831=ORIENTED_EDGE('',*,*,#3273,.T.);
#4832=ORIENTED_EDGE('',*,*,#3277,.T.);
#4833=ORIENTED_EDGE('',*,*,#3285,.F.);
#4834=ORIENTED_EDGE('',*,*,#3403,.F.);
#4835=ORIENTED_EDGE('',*,*,#3397,.T.);
#4836=ORIENTED_EDGE('',*,*,#3401,.T.);
#4837=ORIENTED_EDGE('',*,*,#3386,.F.);
#4838=ORIENTED_EDGE('',*,*,#3380,.F.);
#4839=ORIENTED_EDGE('',*,*,#3373,.T.);
#4840=ORIENTED_EDGE('',*,*,#3377,.T.);
#4841=ORIENTED_EDGE('',*,*,#3385,.F.);
#4842=ORIENTED_EDGE('',*,*,#3395,.F.);
#4843=ORIENTED_EDGE('',*,*,#3389,.T.);
#4844=ORIENTED_EDGE('',*,*,#3393,.T.);
#4845=ORIENTED_EDGE('',*,*,#3370,.F.);
#4846=ORIENTED_EDGE('',*,*,#3367,.F.);
#4847=ORIENTED_EDGE('',*,*,#3361,.T.);
#4848=ORIENTED_EDGE('',*,*,#3365,.T.);
#4849=ORIENTED_EDGE('',*,*,#3334,.F.);
#4850=ORIENTED_EDGE('',*,*,#3328,.F.);
#4851=ORIENTED_EDGE('',*,*,#3321,.T.);
#4852=ORIENTED_EDGE('',*,*,#3325,.T.);
#4853=ORIENTED_EDGE('',*,*,#3333,.F.);
#4854=ORIENTED_EDGE('',*,*,#3344,.F.);
#4855=ORIENTED_EDGE('',*,*,#3337,.T.);
#4856=ORIENTED_EDGE('',*,*,#3341,.T.);
#4857=ORIENTED_EDGE('',*,*,#3348,.F.);
#4858=ORIENTED_EDGE('',*,*,#3356,.F.);
#4859=ORIENTED_EDGE('',*,*,#3349,.T.);
#4860=ORIENTED_EDGE('',*,*,#3353,.T.);
#4861=ORIENTED_EDGE('',*,*,#3423,.F.);
#4862=ORIENTED_EDGE('',*,*,#3483,.F.);
#4863=ORIENTED_EDGE('',*,*,#3430,.F.);
#4864=ORIENTED_EDGE('',*,*,#3413,.T.);
#4865=ORIENTED_EDGE('',*,*,#3417,.F.);
#4866=ORIENTED_EDGE('',*,*,#3429,.F.);
#4867=ORIENTED_EDGE('',*,*,#3433,.T.);
#4868=ORIENTED_EDGE('',*,*,#3424,.F.);
#4869=ORIENTED_EDGE('',*,*,#3435,.F.);
#4870=ORIENTED_EDGE('',*,*,#3444,.F.);
#4871=ORIENTED_EDGE('',*,*,#3445,.T.);
#4872=ORIENTED_EDGE('',*,*,#3439,.F.);
#4873=ORIENTED_EDGE('',*,*,#3447,.F.);
#4874=ORIENTED_EDGE('',*,*,#3456,.F.);
#4875=ORIENTED_EDGE('',*,*,#3457,.T.);
#4876=ORIENTED_EDGE('',*,*,#3451,.F.);
#4877=ORIENTED_EDGE('',*,*,#3459,.F.);
#4878=ORIENTED_EDGE('',*,*,#3468,.F.);
#4879=ORIENTED_EDGE('',*,*,#3469,.T.);
#4880=ORIENTED_EDGE('',*,*,#3463,.F.);
#4881=ORIENTED_EDGE('',*,*,#3485,.F.);
#4882=ORIENTED_EDGE('',*,*,#3471,.F.);
#4883=ORIENTED_EDGE('',*,*,#3480,.F.);
#4884=ORIENTED_EDGE('',*,*,#3481,.T.);
#4885=ORIENTED_EDGE('',*,*,#3475,.F.);
#4886=ORIENTED_EDGE('',*,*,#3488,.F.);
#4887=ORIENTED_EDGE('',*,*,#3489,.T.);
#4888=ORIENTED_EDGE('',*,*,#3490,.F.);
#4889=ORIENTED_EDGE('',*,*,#3489,.F.);
#4890=ORIENTED_EDGE('',*,*,#3491,.T.);
#4891=ORIENTED_EDGE('',*,*,#3488,.T.);
#4892=ORIENTED_EDGE('',*,*,#3492,.T.);
#4893=ORIENTED_EDGE('',*,*,#3493,.T.);
#4894=ORIENTED_EDGE('',*,*,#3494,.T.);
#4895=ORIENTED_EDGE('',*,*,#3495,.T.);
#4896=ORIENTED_EDGE('',*,*,#3496,.T.);
#4897=ORIENTED_EDGE('',*,*,#3497,.T.);
#4898=ORIENTED_EDGE('',*,*,#3498,.T.);
#4899=ORIENTED_EDGE('',*,*,#3499,.T.);
#4900=ORIENTED_EDGE('',*,*,#3500,.T.);
#4901=ORIENTED_EDGE('',*,*,#3501,.T.);
#4902=ORIENTED_EDGE('',*,*,#3502,.T.);
#4903=ORIENTED_EDGE('',*,*,#3503,.T.);
#4904=ORIENTED_EDGE('',*,*,#3504,.T.);
#4905=ORIENTED_EDGE('',*,*,#3505,.T.);
#4906=ORIENTED_EDGE('',*,*,#3506,.T.);
#4907=ORIENTED_EDGE('',*,*,#3507,.T.);
#4908=ORIENTED_EDGE('',*,*,#3490,.T.);
#4909=ORIENTED_EDGE('',*,*,#3508,.F.);
#4910=ORIENTED_EDGE('',*,*,#3493,.F.);
#4911=ORIENTED_EDGE('',*,*,#3509,.T.);
#4912=ORIENTED_EDGE('',*,*,#3510,.T.);
#4913=ORIENTED_EDGE('',*,*,#3511,.T.);
#4914=ORIENTED_EDGE('',*,*,#3512,.T.);
#4915=ORIENTED_EDGE('',*,*,#3505,.F.);
#4916=ORIENTED_EDGE('',*,*,#3513,.F.);
#4917=ORIENTED_EDGE('',*,*,#3514,.T.);
#4918=ORIENTED_EDGE('',*,*,#3515,.T.);
#4919=ORIENTED_EDGE('',*,*,#3506,.F.);
#4920=ORIENTED_EDGE('',*,*,#3512,.F.);
#4921=ORIENTED_EDGE('',*,*,#3516,.F.);
#4922=ORIENTED_EDGE('',*,*,#3517,.T.);
#4923=ORIENTED_EDGE('',*,*,#3507,.F.);
#4924=ORIENTED_EDGE('',*,*,#3515,.F.);
#4925=ORIENTED_EDGE('',*,*,#3518,.F.);
#4926=ORIENTED_EDGE('',*,*,#3519,.F.);
#4927=ORIENTED_EDGE('',*,*,#3513,.T.);
#4928=ORIENTED_EDGE('',*,*,#3504,.F.);
#4929=ORIENTED_EDGE('',*,*,#3509,.F.);
#4930=ORIENTED_EDGE('',*,*,#3492,.F.);
#4931=ORIENTED_EDGE('',*,*,#3517,.F.);
#4932=ORIENTED_EDGE('',*,*,#3520,.T.);
#4933=ORIENTED_EDGE('',*,*,#3510,.F.);
#4934=ORIENTED_EDGE('',*,*,#3520,.F.);
#4935=ORIENTED_EDGE('',*,*,#3516,.T.);
#4936=ORIENTED_EDGE('',*,*,#3514,.F.);
#4937=ORIENTED_EDGE('',*,*,#3511,.F.);
#4938=ORIENTED_EDGE('',*,*,#3519,.T.);
#4939=ORIENTED_EDGE('',*,*,#3521,.T.);
#4940=ORIENTED_EDGE('',*,*,#3522,.T.);
#4941=ORIENTED_EDGE('',*,*,#3523,.F.);
#4942=ORIENTED_EDGE('',*,*,#3524,.T.);
#4943=ORIENTED_EDGE('',*,*,#3525,.F.);
#4944=ORIENTED_EDGE('',*,*,#3526,.F.);
#4945=ORIENTED_EDGE('',*,*,#3527,.T.);
#4946=ORIENTED_EDGE('',*,*,#3528,.F.);
#4947=ORIENTED_EDGE('',*,*,#3529,.F.);
#4948=ORIENTED_EDGE('',*,*,#3530,.F.);
#4949=ORIENTED_EDGE('',*,*,#3531,.F.);
#4950=ORIENTED_EDGE('',*,*,#3518,.T.);
#4951=ORIENTED_EDGE('',*,*,#3503,.F.);
#4952=ORIENTED_EDGE('',*,*,#3532,.F.);
#4953=ORIENTED_EDGE('',*,*,#3521,.F.);
#4954=ORIENTED_EDGE('',*,*,#3532,.T.);
#4955=ORIENTED_EDGE('',*,*,#3502,.F.);
#4956=ORIENTED_EDGE('',*,*,#3533,.F.);
#4957=ORIENTED_EDGE('',*,*,#3522,.F.);
#4958=ORIENTED_EDGE('',*,*,#3531,.T.);
#4959=ORIENTED_EDGE('',*,*,#3534,.T.);
#4960=ORIENTED_EDGE('',*,*,#3491,.F.);
#4961=ORIENTED_EDGE('',*,*,#3534,.F.);
#4962=ORIENTED_EDGE('',*,*,#3523,.T.);
#4963=ORIENTED_EDGE('',*,*,#3533,.T.);
#4964=ORIENTED_EDGE('',*,*,#3501,.F.);
#4965=ORIENTED_EDGE('',*,*,#3535,.F.);
#4966=ORIENTED_EDGE('',*,*,#3524,.F.);
#4967=ORIENTED_EDGE('',*,*,#3535,.T.);
#4968=ORIENTED_EDGE('',*,*,#3500,.F.);
#4969=ORIENTED_EDGE('',*,*,#3536,.F.);
#4970=ORIENTED_EDGE('',*,*,#3525,.T.);
#4971=ORIENTED_EDGE('',*,*,#3536,.T.);
#4972=ORIENTED_EDGE('',*,*,#3499,.F.);
#4973=ORIENTED_EDGE('',*,*,#3537,.F.);
#4974=ORIENTED_EDGE('',*,*,#3526,.T.);
#4975=ORIENTED_EDGE('',*,*,#3537,.T.);
#4976=ORIENTED_EDGE('',*,*,#3498,.F.);
#4977=ORIENTED_EDGE('',*,*,#3538,.F.);
#4978=ORIENTED_EDGE('',*,*,#3527,.F.);
#4979=ORIENTED_EDGE('',*,*,#3538,.T.);
#4980=ORIENTED_EDGE('',*,*,#3497,.F.);
#4981=ORIENTED_EDGE('',*,*,#3539,.F.);
#4982=ORIENTED_EDGE('',*,*,#3528,.T.);
#4983=ORIENTED_EDGE('',*,*,#3539,.T.);
#4984=ORIENTED_EDGE('',*,*,#3496,.F.);
#4985=ORIENTED_EDGE('',*,*,#3540,.F.);
#4986=ORIENTED_EDGE('',*,*,#3529,.T.);
#4987=ORIENTED_EDGE('',*,*,#3540,.T.);
#4988=ORIENTED_EDGE('',*,*,#3495,.F.);
#4989=ORIENTED_EDGE('',*,*,#3541,.F.);
#4990=ORIENTED_EDGE('',*,*,#3508,.T.);
#4991=ORIENTED_EDGE('',*,*,#3530,.T.);
#4992=ORIENTED_EDGE('',*,*,#3541,.T.);
#4993=ORIENTED_EDGE('',*,*,#3494,.F.);
#4994=ORIENTED_EDGE('',*,*,#3542,.F.);
#4995=ORIENTED_EDGE('',*,*,#3543,.T.);
#4996=ORIENTED_EDGE('',*,*,#3544,.T.);
#4997=ORIENTED_EDGE('',*,*,#3543,.F.);
#4998=ORIENTED_EDGE('',*,*,#3545,.F.);
#4999=ORIENTED_EDGE('',*,*,#3546,.T.);
#5000=ORIENTED_EDGE('',*,*,#3547,.T.);
#5001=ORIENTED_EDGE('',*,*,#3546,.F.);
#5002=ORIENTED_EDGE('',*,*,#3548,.F.);
#5003=ORIENTED_EDGE('',*,*,#3549,.F.);
#5004=ORIENTED_EDGE('',*,*,#3550,.T.);
#5005=ORIENTED_EDGE('',*,*,#3551,.T.);
#5006=ORIENTED_EDGE('',*,*,#3550,.F.);
#5007=ORIENTED_EDGE('',*,*,#3548,.T.);
#5008=ORIENTED_EDGE('',*,*,#3549,.T.);
#5009=ORIENTED_EDGE('',*,*,#3552,.T.);
#5010=ORIENTED_EDGE('',*,*,#3553,.F.);
#5011=ORIENTED_EDGE('',*,*,#3552,.F.);
#5012=ORIENTED_EDGE('',*,*,#3554,.F.);
#5013=ORIENTED_EDGE('',*,*,#3555,.T.);
#5014=ORIENTED_EDGE('',*,*,#3556,.T.);
#5015=ORIENTED_EDGE('',*,*,#3555,.F.);
#5016=ORIENTED_EDGE('',*,*,#3557,.F.);
#5017=ORIENTED_EDGE('',*,*,#3558,.T.);
#5018=ORIENTED_EDGE('',*,*,#3554,.T.);
#5019=ORIENTED_EDGE('',*,*,#3558,.F.);
#5020=ORIENTED_EDGE('',*,*,#3559,.F.);
#5021=ORIENTED_EDGE('',*,*,#3560,.T.);
#5022=ORIENTED_EDGE('',*,*,#3557,.T.);
#5023=ORIENTED_EDGE('',*,*,#3560,.F.);
#5024=ORIENTED_EDGE('',*,*,#3544,.F.);
#5025=ORIENTED_EDGE('',*,*,#3561,.T.);
#5026=ORIENTED_EDGE('',*,*,#3562,.T.);
#5027=ORIENTED_EDGE('',*,*,#3561,.F.);
#5028=ORIENTED_EDGE('',*,*,#3559,.T.);
#5029=ORIENTED_EDGE('',*,*,#3562,.F.);
#5030=ORIENTED_EDGE('',*,*,#3556,.F.);
#5031=ORIENTED_EDGE('',*,*,#3553,.T.);
#5032=ORIENTED_EDGE('',*,*,#3545,.T.);
#5033=ORIENTED_EDGE('',*,*,#3551,.F.);
#5034=ORIENTED_EDGE('',*,*,#3547,.F.);
#5035=ORIENTED_EDGE('',*,*,#3542,.T.);
#5036=ORIENTED_EDGE('',*,*,#3563,.T.);
#5037=ORIENTED_EDGE('',*,*,#3564,.T.);
#5038=ORIENTED_EDGE('',*,*,#3565,.F.);
#5039=ORIENTED_EDGE('',*,*,#3564,.F.);
#5040=ORIENTED_EDGE('',*,*,#3566,.T.);
#5041=ORIENTED_EDGE('',*,*,#3563,.F.);
#5042=ORIENTED_EDGE('',*,*,#3567,.T.);
#5043=ORIENTED_EDGE('',*,*,#3568,.T.);
#5044=ORIENTED_EDGE('',*,*,#3567,.F.);
#5045=ORIENTED_EDGE('',*,*,#3566,.F.);
#5046=ORIENTED_EDGE('',*,*,#3568,.F.);
#5047=ORIENTED_EDGE('',*,*,#3569,.T.);
#5048=ORIENTED_EDGE('',*,*,#3570,.T.);
#5049=ORIENTED_EDGE('',*,*,#3569,.F.);
#5050=ORIENTED_EDGE('',*,*,#3571,.F.);
#5051=ORIENTED_EDGE('',*,*,#3572,.T.);
#5052=ORIENTED_EDGE('',*,*,#3573,.T.);
#5053=ORIENTED_EDGE('',*,*,#3572,.F.);
#5054=ORIENTED_EDGE('',*,*,#3574,.F.);
#5055=ORIENTED_EDGE('',*,*,#3575,.T.);
#5056=ORIENTED_EDGE('',*,*,#3576,.T.);
#5057=ORIENTED_EDGE('',*,*,#3575,.F.);
#5058=ORIENTED_EDGE('',*,*,#3576,.F.);
#5059=ORIENTED_EDGE('',*,*,#3577,.T.);
#5060=ORIENTED_EDGE('',*,*,#3578,.T.);
#5061=ORIENTED_EDGE('',*,*,#3577,.F.);
#5062=ORIENTED_EDGE('',*,*,#3578,.F.);
#5063=ORIENTED_EDGE('',*,*,#3579,.T.);
#5064=ORIENTED_EDGE('',*,*,#3580,.T.);
#5065=ORIENTED_EDGE('',*,*,#3579,.F.);
#5066=ORIENTED_EDGE('',*,*,#3581,.F.);
#5067=ORIENTED_EDGE('',*,*,#3582,.T.);
#5068=ORIENTED_EDGE('',*,*,#3583,.T.);
#5069=ORIENTED_EDGE('',*,*,#3582,.F.);
#5070=ORIENTED_EDGE('',*,*,#3583,.F.);
#5071=ORIENTED_EDGE('',*,*,#3584,.T.);
#5072=ORIENTED_EDGE('',*,*,#3585,.T.);
#5073=ORIENTED_EDGE('',*,*,#3584,.F.);
#5074=ORIENTED_EDGE('',*,*,#3585,.F.);
#5075=ORIENTED_EDGE('',*,*,#3586,.T.);
#5076=ORIENTED_EDGE('',*,*,#3587,.T.);
#5077=ORIENTED_EDGE('',*,*,#3586,.F.);
#5078=ORIENTED_EDGE('',*,*,#3580,.F.);
#5079=ORIENTED_EDGE('',*,*,#3581,.T.);
#5080=ORIENTED_EDGE('',*,*,#3573,.F.);
#5081=ORIENTED_EDGE('',*,*,#3574,.T.);
#5082=ORIENTED_EDGE('',*,*,#3571,.T.);
#5083=ORIENTED_EDGE('',*,*,#3570,.F.);
#5084=ORIENTED_EDGE('',*,*,#3565,.T.);
#5085=ORIENTED_EDGE('',*,*,#3587,.F.);
#5086=ORIENTED_EDGE('',*,*,#3588,.F.);
#5087=ORIENTED_EDGE('',*,*,#3589,.T.);
#5088=ORIENTED_EDGE('',*,*,#3590,.T.);
#5089=ORIENTED_EDGE('',*,*,#3589,.F.);
#5090=ORIENTED_EDGE('',*,*,#3591,.F.);
#5091=ORIENTED_EDGE('',*,*,#3592,.T.);
#5092=ORIENTED_EDGE('',*,*,#3593,.T.);
#5093=ORIENTED_EDGE('',*,*,#3592,.F.);
#5094=ORIENTED_EDGE('',*,*,#3594,.F.);
#5095=ORIENTED_EDGE('',*,*,#3595,.T.);
#5096=ORIENTED_EDGE('',*,*,#3591,.T.);
#5097=ORIENTED_EDGE('',*,*,#3595,.F.);
#5098=ORIENTED_EDGE('',*,*,#3596,.F.);
#5099=ORIENTED_EDGE('',*,*,#3597,.T.);
#5100=ORIENTED_EDGE('',*,*,#3594,.T.);
#5101=ORIENTED_EDGE('',*,*,#3597,.F.);
#5102=ORIENTED_EDGE('',*,*,#3598,.F.);
#5103=ORIENTED_EDGE('',*,*,#3599,.T.);
#5104=ORIENTED_EDGE('',*,*,#3600,.T.);
#5105=ORIENTED_EDGE('',*,*,#3599,.F.);
#5106=ORIENTED_EDGE('',*,*,#3601,.F.);
#5107=ORIENTED_EDGE('',*,*,#3602,.T.);
#5108=ORIENTED_EDGE('',*,*,#3598,.T.);
#5109=ORIENTED_EDGE('',*,*,#3602,.F.);
#5110=ORIENTED_EDGE('',*,*,#3603,.F.);
#5111=ORIENTED_EDGE('',*,*,#3604,.T.);
#5112=ORIENTED_EDGE('',*,*,#3601,.T.);
#5113=ORIENTED_EDGE('',*,*,#3604,.F.);
#5114=ORIENTED_EDGE('',*,*,#3605,.F.);
#5115=ORIENTED_EDGE('',*,*,#3606,.T.);
#5116=ORIENTED_EDGE('',*,*,#3607,.T.);
#5117=ORIENTED_EDGE('',*,*,#3606,.F.);
#5118=ORIENTED_EDGE('',*,*,#3608,.F.);
#5119=ORIENTED_EDGE('',*,*,#3609,.T.);
#5120=ORIENTED_EDGE('',*,*,#3605,.T.);
#5121=ORIENTED_EDGE('',*,*,#3609,.F.);
#5122=ORIENTED_EDGE('',*,*,#3610,.F.);
#5123=ORIENTED_EDGE('',*,*,#3611,.T.);
#5124=ORIENTED_EDGE('',*,*,#3608,.T.);
#5125=ORIENTED_EDGE('',*,*,#3611,.F.);
#5126=ORIENTED_EDGE('',*,*,#3612,.F.);
#5127=ORIENTED_EDGE('',*,*,#3613,.T.);
#5128=ORIENTED_EDGE('',*,*,#3614,.T.);
#5129=ORIENTED_EDGE('',*,*,#3613,.F.);
#5130=ORIENTED_EDGE('',*,*,#3615,.F.);
#5131=ORIENTED_EDGE('',*,*,#3616,.T.);
#5132=ORIENTED_EDGE('',*,*,#3612,.T.);
#5133=ORIENTED_EDGE('',*,*,#3616,.F.);
#5134=ORIENTED_EDGE('',*,*,#3615,.T.);
#5135=ORIENTED_EDGE('',*,*,#3590,.F.);
#5136=ORIENTED_EDGE('',*,*,#3610,.T.);
#5137=ORIENTED_EDGE('',*,*,#3614,.F.);
#5138=ORIENTED_EDGE('',*,*,#3603,.T.);
#5139=ORIENTED_EDGE('',*,*,#3607,.F.);
#5140=ORIENTED_EDGE('',*,*,#3600,.F.);
#5141=ORIENTED_EDGE('',*,*,#3596,.T.);
#5142=ORIENTED_EDGE('',*,*,#3593,.F.);
#5143=ORIENTED_EDGE('',*,*,#3588,.T.);
#5144=ORIENTED_EDGE('',*,*,#3617,.T.);
#5145=ORIENTED_EDGE('',*,*,#3618,.T.);
#5146=ORIENTED_EDGE('',*,*,#3619,.F.);
#5147=ORIENTED_EDGE('',*,*,#3618,.F.);
#5148=ORIENTED_EDGE('',*,*,#3620,.T.);
#5149=ORIENTED_EDGE('',*,*,#3621,.T.);
#5150=ORIENTED_EDGE('',*,*,#3622,.F.);
#5151=ORIENTED_EDGE('',*,*,#3621,.F.);
#5152=ORIENTED_EDGE('',*,*,#3623,.T.);
#5153=ORIENTED_EDGE('',*,*,#3624,.T.);
#5154=ORIENTED_EDGE('',*,*,#3620,.F.);
#5155=ORIENTED_EDGE('',*,*,#3624,.F.);
#5156=ORIENTED_EDGE('',*,*,#3625,.T.);
#5157=ORIENTED_EDGE('',*,*,#3626,.T.);
#5158=ORIENTED_EDGE('',*,*,#3623,.F.);
#5159=ORIENTED_EDGE('',*,*,#3626,.F.);
#5160=ORIENTED_EDGE('',*,*,#3627,.T.);
#5161=ORIENTED_EDGE('',*,*,#3628,.T.);
#5162=ORIENTED_EDGE('',*,*,#3629,.F.);
#5163=ORIENTED_EDGE('',*,*,#3628,.F.);
#5164=ORIENTED_EDGE('',*,*,#3630,.T.);
#5165=ORIENTED_EDGE('',*,*,#3631,.T.);
#5166=ORIENTED_EDGE('',*,*,#3627,.F.);
#5167=ORIENTED_EDGE('',*,*,#3631,.F.);
#5168=ORIENTED_EDGE('',*,*,#3632,.T.);
#5169=ORIENTED_EDGE('',*,*,#3633,.T.);
#5170=ORIENTED_EDGE('',*,*,#3630,.F.);
#5171=ORIENTED_EDGE('',*,*,#3633,.F.);
#5172=ORIENTED_EDGE('',*,*,#3634,.T.);
#5173=ORIENTED_EDGE('',*,*,#3635,.T.);
#5174=ORIENTED_EDGE('',*,*,#3636,.F.);
#5175=ORIENTED_EDGE('',*,*,#3635,.F.);
#5176=ORIENTED_EDGE('',*,*,#3637,.T.);
#5177=ORIENTED_EDGE('',*,*,#3638,.T.);
#5178=ORIENTED_EDGE('',*,*,#3634,.F.);
#5179=ORIENTED_EDGE('',*,*,#3638,.F.);
#5180=ORIENTED_EDGE('',*,*,#3639,.T.);
#5181=ORIENTED_EDGE('',*,*,#3640,.T.);
#5182=ORIENTED_EDGE('',*,*,#3637,.F.);
#5183=ORIENTED_EDGE('',*,*,#3640,.F.);
#5184=ORIENTED_EDGE('',*,*,#3641,.T.);
#5185=ORIENTED_EDGE('',*,*,#3642,.T.);
#5186=ORIENTED_EDGE('',*,*,#3643,.F.);
#5187=ORIENTED_EDGE('',*,*,#3642,.F.);
#5188=ORIENTED_EDGE('',*,*,#3644,.T.);
#5189=ORIENTED_EDGE('',*,*,#3645,.T.);
#5190=ORIENTED_EDGE('',*,*,#3641,.F.);
#5191=ORIENTED_EDGE('',*,*,#3645,.F.);
#5192=ORIENTED_EDGE('',*,*,#3644,.F.);
#5193=ORIENTED_EDGE('',*,*,#3619,.T.);
#5194=ORIENTED_EDGE('',*,*,#3639,.F.);
#5195=ORIENTED_EDGE('',*,*,#3643,.T.);
#5196=ORIENTED_EDGE('',*,*,#3632,.F.);
#5197=ORIENTED_EDGE('',*,*,#3636,.T.);
#5198=ORIENTED_EDGE('',*,*,#3629,.T.);
#5199=ORIENTED_EDGE('',*,*,#3625,.F.);
#5200=ORIENTED_EDGE('',*,*,#3622,.T.);
#5201=ORIENTED_EDGE('',*,*,#3617,.F.);
#5202=CYLINDRICAL_SURFACE('',#5721,4.8);
#5203=CYLINDRICAL_SURFACE('',#5724,4.872);
#5204=CYLINDRICAL_SURFACE('',#5727,4.8);
#5205=CYLINDRICAL_SURFACE('',#5737,6.);
#5206=CYLINDRICAL_SURFACE('',#5752,3.1184375);
#5207=CYLINDRICAL_SURFACE('',#5757,3.272);
#5208=CYLINDRICAL_SURFACE('',#5764,3.1184375);
#5209=CYLINDRICAL_SURFACE('',#5772,2.);
#5210=CYLINDRICAL_SURFACE('',#5781,3.2);
#5211=CYLINDRICAL_SURFACE('',#5822,3.2);
#5212=CYLINDRICAL_SURFACE('',#5885,1.78525000000062);
#5213=CYLINDRICAL_SURFACE('',#5889,1.954);
#5214=CYLINDRICAL_SURFACE('',#5891,2.);
#5215=CYLINDRICAL_SURFACE('',#5894,2.);
#5216=CYLINDRICAL_SURFACE('',#5897,6.00000000000001);
#5217=CYLINDRICAL_SURFACE('',#5900,7.00000000000001);
#5218=CYLINDRICAL_SURFACE('',#5906,6.00000000000001);
#5219=CYLINDRICAL_SURFACE('',#5909,7.00000000000001);
#5220=CYLINDRICAL_SURFACE('',#5920,1.99999999999999);
#5221=CYLINDRICAL_SURFACE('',#5923,2.99999999999999);
#5222=CYLINDRICAL_SURFACE('',#5934,0.770000000000005);
#5223=CYLINDRICAL_SURFACE('',#5941,0.770000000000005);
#5224=CYLINDRICAL_SURFACE('',#5945,1.99999999999999);
#5225=CYLINDRICAL_SURFACE('',#5952,25.5);
#5226=CYLINDRICAL_SURFACE('',#5955,25.5);
#5227=CYLINDRICAL_SURFACE('',#5961,25.5);
#5228=CYLINDRICAL_SURFACE('',#5967,25.5);
#5229=CYLINDRICAL_SURFACE('',#5973,25.5);
#5230=CYLINDRICAL_SURFACE('',#5979,25.5);
#5231=CYLINDRICAL_SURFACE('',#5985,25.5);
#5232=CYLINDRICAL_SURFACE('',#5988,25.5);
#5233=CYLINDRICAL_SURFACE('',#5997,25.5);
#5234=CYLINDRICAL_SURFACE('',#6003,25.5);
#5235=CYLINDRICAL_SURFACE('',#6006,25.5);
#5236=CYLINDRICAL_SURFACE('',#6012,25.5);
#5237=CYLINDRICAL_SURFACE('',#6015,25.5);
#5238=CYLINDRICAL_SURFACE('',#6027,25.5);
#5239=CYLINDRICAL_SURFACE('',#6033,25.5);
#5240=CYLINDRICAL_SURFACE('',#6039,25.5);
#5241=CYLINDRICAL_SURFACE('',#6042,25.5);
#5242=CYLINDRICAL_SURFACE('',#6048,25.5);
#5243=CYLINDRICAL_SURFACE('',#6054,25.5);
#5244=CYLINDRICAL_SURFACE('',#6063,25.5);
#5245=CYLINDRICAL_SURFACE('',#6066,25.5);
#5246=CYLINDRICAL_SURFACE('',#6075,25.5);
#5247=CYLINDRICAL_SURFACE('',#6078,25.5);
#5248=CYLINDRICAL_SURFACE('',#6087,25.5);
#5249=CYLINDRICAL_SURFACE('',#6090,25.5);
#5250=CYLINDRICAL_SURFACE('',#6096,25.5);
#5251=CYLINDRICAL_SURFACE('',#6102,25.5);
#5252=CYLINDRICAL_SURFACE('',#6108,25.5);
#5253=CYLINDRICAL_SURFACE('',#6114,25.5);
#5254=CYLINDRICAL_SURFACE('',#6117,25.5);
#5255=CYLINDRICAL_SURFACE('',#6131,22.);
#5256=CYLINDRICAL_SURFACE('',#6134,22.);
#5257=CYLINDRICAL_SURFACE('',#6137,7.00000000000001);
#5258=CYLINDRICAL_SURFACE('',#6140,7.00000000000001);
#5259=CYLINDRICAL_SURFACE('',#6145,22.);
#5260=CYLINDRICAL_SURFACE('',#6148,7.00000000000001);
#5261=CYLINDRICAL_SURFACE('',#6153,22.);
#5262=CYLINDRICAL_SURFACE('',#6156,7.00000000000001);
#5263=CYLINDRICAL_SURFACE('',#6161,22.);
#5264=CYLINDRICAL_SURFACE('',#6164,7.00000000000001);
#5265=CYLINDRICAL_SURFACE('',#6169,22.);
#5266=CYLINDRICAL_SURFACE('',#6172,7.00000000000001);
#5267=CYLINDRICAL_SURFACE('',#6177,6.00000000000001);
#5268=CYLINDRICAL_SURFACE('',#6183,3.37715398312954);
#5269=CYLINDRICAL_SURFACE('',#6196,26.714151341222);
#5270=CYLINDRICAL_SURFACE('',#6199,23.514151341222);
#5271=CYLINDRICAL_SURFACE('',#6211,6.00000000000001);
#5272=CYLINDRICAL_SURFACE('',#6212,7.00000000000001);
#5273=CYLINDRICAL_SURFACE('',#6214,32.2155772121003);
#5274=CYLINDRICAL_SURFACE('',#6216,29.0155772121003);
#5275=CYLINDRICAL_SURFACE('',#6218,7.00000000000001);
#5276=CYLINDRICAL_SURFACE('',#6221,4.8);
#5277=CYLINDRICAL_SURFACE('',#6224,4.872);
#5278=CYLINDRICAL_SURFACE('',#6227,4.8);
#5279=CYLINDRICAL_SURFACE('',#6237,6.);
#5280=CYLINDRICAL_SURFACE('',#6252,3.1184375);
#5281=CYLINDRICAL_SURFACE('',#6257,3.272);
#5282=CYLINDRICAL_SURFACE('',#6264,3.1184375);
#5283=CYLINDRICAL_SURFACE('',#6272,2.);
#5284=CYLINDRICAL_SURFACE('',#6281,3.2);
#5285=CYLINDRICAL_SURFACE('',#6322,3.2);
#5286=ADVANCED_FACE('',(#407),#5202,.F.);
#5287=ADVANCED_FACE('',(#408),#5203,.F.);
#5288=ADVANCED_FACE('',(#409),#5204,.F.);
#5289=ADVANCED_FACE('',(#410),#380,.F.);
#5290=ADVANCED_FACE('',(#411),#337,.T.);
#5291=ADVANCED_FACE('',(#412),#5205,.T.);
#5292=ADVANCED_FACE('',(#413),#338,.T.);
#5293=ADVANCED_FACE('',(#414),#381,.F.);
#5294=ADVANCED_FACE('',(#415,#96),#161,.F.);
#5295=ADVANCED_FACE('',(#416,#97),#162,.F.);
#5296=ADVANCED_FACE('',(#417,#98),#163,.F.);
#5297=ADVANCED_FACE('',(#418,#99),#164,.F.);
#5298=ADVANCED_FACE('',(#419),#382,.T.);
#5299=ADVANCED_FACE('',(#420),#5206,.T.);
#5300=ADVANCED_FACE('',(#421),#339,.F.);
#5301=ADVANCED_FACE('',(#422),#5207,.T.);
#5302=ADVANCED_FACE('',(#423),#340,.F.);
#5303=ADVANCED_FACE('',(#424),#5208,.T.);
#5304=ADVANCED_FACE('',(#425),#383,.T.);
#5305=ADVANCED_FACE('',(#426),#341,.T.);
#5306=ADVANCED_FACE('',(#427),#5209,.F.);
#5307=ADVANCED_FACE('',(#428),#342,.T.);
#5308=ADVANCED_FACE('',(#429,#100),#165,.F.);
#5309=ADVANCED_FACE('',(#430,#101),#166,.F.);
#5310=ADVANCED_FACE('',(#431,#102),#167,.F.);
#5311=ADVANCED_FACE('',(#432,#103),#168,.F.);
#5312=ADVANCED_FACE('',(#433),#5210,.F.);
#5313=ADVANCED_FACE('',(#434),#343,.T.);
#5314=ADVANCED_FACE('',(#435),#384,.T.);
#5315=ADVANCED_FACE('',(#436),#344,.F.);
#5316=ADVANCED_FACE('',(#437),#345,.F.);
#5317=ADVANCED_FACE('',(#438),#385,.F.);
#5318=ADVANCED_FACE('',(#439),#346,.F.);
#5319=ADVANCED_FACE('',(#440),#347,.T.);
#5320=ADVANCED_FACE('',(#441),#386,.T.);
#5321=ADVANCED_FACE('',(#442),#348,.T.);
#5322=ADVANCED_FACE('',(#443),#349,.T.);
#5323=ADVANCED_FACE('',(#444),#387,.F.);
#5324=ADVANCED_FACE('',(#445,#104),#169,.F.);
#5325=ADVANCED_FACE('',(#446,#105),#170,.F.);
#5326=ADVANCED_FACE('',(#447,#106),#171,.T.);
#5327=ADVANCED_FACE('',(#448,#107),#172,.T.);
#5328=ADVANCED_FACE('',(#449,#108),#173,.T.);
#5329=ADVANCED_FACE('',(#450),#5211,.F.);
#5330=ADVANCED_FACE('',(#451),#350,.T.);
#5331=ADVANCED_FACE('',(#452),#388,.T.);
#5332=ADVANCED_FACE('',(#453),#351,.F.);
#5333=ADVANCED_FACE('',(#454),#352,.F.);
#5334=ADVANCED_FACE('',(#455),#389,.F.);
#5335=ADVANCED_FACE('',(#456),#353,.F.);
#5336=ADVANCED_FACE('',(#457),#354,.T.);
#5337=ADVANCED_FACE('',(#458),#390,.T.);
#5338=ADVANCED_FACE('',(#459),#355,.T.);
#5339=ADVANCED_FACE('',(#460),#356,.T.);
#5340=ADVANCED_FACE('',(#461),#391,.F.);
#5341=ADVANCED_FACE('',(#462,#109),#174,.F.);
#5342=ADVANCED_FACE('',(#463,#110),#175,.F.);
#5343=ADVANCED_FACE('',(#464,#111),#176,.T.);
#5344=ADVANCED_FACE('',(#465,#112),#177,.T.);
#5345=ADVANCED_FACE('',(#466,#113),#178,.T.);
#5346=ADVANCED_FACE('',(#467),#392,.T.);
#5347=ADVANCED_FACE('',(#468),#179,.F.);
#5348=ADVANCED_FACE('',(#469),#180,.F.);
#5349=ADVANCED_FACE('',(#470),#181,.T.);
#5350=ADVANCED_FACE('',(#471),#182,.T.);
#5351=ADVANCED_FACE('',(#472),#183,.T.);
#5352=ADVANCED_FACE('',(#473),#357,.T.);
#5353=ADVANCED_FACE('',(#474),#393,.T.);
#5354=ADVANCED_FACE('',(#475),#184,.T.);
#5355=ADVANCED_FACE('',(#476,#114),#185,.T.);
#5356=ADVANCED_FACE('',(#477),#5212,.T.);
#5357=ADVANCED_FACE('',(#478),#394,.T.);
#5358=ADVANCED_FACE('',(#479),#5213,.T.);
#5359=ADVANCED_FACE('',(#480),#5214,.F.);
#5360=ADVANCED_FACE('',(#481),#5215,.F.);
#5361=ADVANCED_FACE('',(#482),#5216,.F.);
#5362=ADVANCED_FACE('',(#483),#5217,.T.);
#5363=ADVANCED_FACE('',(#484,#115),#186,.T.);
#5364=ADVANCED_FACE('',(#485,#116,#117),#187,.F.);
#5365=ADVANCED_FACE('',(#486),#5218,.F.);
#5366=ADVANCED_FACE('',(#487),#5219,.T.);
#5367=ADVANCED_FACE('',(#488,#118),#188,.T.);
#5368=ADVANCED_FACE('',(#489,#119),#189,.F.);
#5369=ADVANCED_FACE('',(#490),#190,.T.);
#5370=ADVANCED_FACE('',(#491),#191,.T.);
#5371=ADVANCED_FACE('',(#492),#192,.T.);
#5372=ADVANCED_FACE('',(#493),#193,.T.);
#5373=ADVANCED_FACE('',(#494,#120,#121),#194,.T.);
#5374=ADVANCED_FACE('',(#495,#122),#195,.F.);
#5375=ADVANCED_FACE('',(#496),#5220,.F.);
#5376=ADVANCED_FACE('',(#497),#5221,.T.);
#5377=ADVANCED_FACE('',(#498,#123),#196,.T.);
#5378=ADVANCED_FACE('',(#499,#124),#197,.F.);
#5379=ADVANCED_FACE('',(#500),#358,.T.);
#5380=ADVANCED_FACE('',(#501),#5222,.T.);
#5381=ADVANCED_FACE('',(#502),#198,.T.);
#5382=ADVANCED_FACE('',(#503),#359,.T.);
#5383=ADVANCED_FACE('',(#504),#5223,.T.);
#5384=ADVANCED_FACE('',(#505),#199,.F.);
#5385=ADVANCED_FACE('',(#506),#200,.F.);
#5386=ADVANCED_FACE('',(#507,#125),#5224,.T.);
#5387=ADVANCED_FACE('',(#508),#201,.T.);
#5388=ADVANCED_FACE('',(#509),#202,.T.);
#5389=ADVANCED_FACE('',(#510),#203,.T.);
#5390=ADVANCED_FACE('',(#511),#204,.T.);
#5391=ADVANCED_FACE('',(#512),#5225,.T.);
#5392=ADVANCED_FACE('',(#513),#5226,.T.);
#5393=ADVANCED_FACE('',(#514),#205,.T.);
#5394=ADVANCED_FACE('',(#515),#206,.T.);
#5395=ADVANCED_FACE('',(#516),#207,.T.);
#5396=ADVANCED_FACE('',(#517),#5227,.T.);
#5397=ADVANCED_FACE('',(#518),#208,.T.);
#5398=ADVANCED_FACE('',(#519),#209,.T.);
#5399=ADVANCED_FACE('',(#520),#210,.T.);
#5400=ADVANCED_FACE('',(#521),#5228,.T.);
#5401=ADVANCED_FACE('',(#522),#211,.T.);
#5402=ADVANCED_FACE('',(#523),#212,.T.);
#5403=ADVANCED_FACE('',(#524),#213,.T.);
#5404=ADVANCED_FACE('',(#525),#5229,.T.);
#5405=ADVANCED_FACE('',(#526),#214,.T.);
#5406=ADVANCED_FACE('',(#527),#215,.T.);
#5407=ADVANCED_FACE('',(#528),#216,.T.);
#5408=ADVANCED_FACE('',(#529),#5230,.T.);
#5409=ADVANCED_FACE('',(#530),#217,.T.);
#5410=ADVANCED_FACE('',(#531),#218,.T.);
#5411=ADVANCED_FACE('',(#532),#219,.T.);
#5412=ADVANCED_FACE('',(#533),#5231,.T.);
#5413=ADVANCED_FACE('',(#534),#5232,.T.);
#5414=ADVANCED_FACE('',(#535),#220,.T.);
#5415=ADVANCED_FACE('',(#536),#221,.T.);
#5416=ADVANCED_FACE('',(#537),#222,.T.);
#5417=ADVANCED_FACE('',(#538),#223,.T.);
#5418=ADVANCED_FACE('',(#539),#224,.T.);
#5419=ADVANCED_FACE('',(#540),#225,.T.);
#5420=ADVANCED_FACE('',(#541),#5233,.T.);
#5421=ADVANCED_FACE('',(#542),#226,.T.);
#5422=ADVANCED_FACE('',(#543),#227,.T.);
#5423=ADVANCED_FACE('',(#544),#228,.T.);
#5424=ADVANCED_FACE('',(#545),#5234,.T.);
#5425=ADVANCED_FACE('',(#546),#5235,.T.);
#5426=ADVANCED_FACE('',(#547),#229,.T.);
#5427=ADVANCED_FACE('',(#548),#230,.T.);
#5428=ADVANCED_FACE('',(#549),#231,.T.);
#5429=ADVANCED_FACE('',(#550),#5236,.T.);
#5430=ADVANCED_FACE('',(#551),#5237,.T.);
#5431=ADVANCED_FACE('',(#552),#232,.T.);
#5432=ADVANCED_FACE('',(#553),#233,.T.);
#5433=ADVANCED_FACE('',(#554),#234,.T.);
#5434=ADVANCED_FACE('',(#555),#235,.T.);
#5435=ADVANCED_FACE('',(#556),#236,.T.);
#5436=ADVANCED_FACE('',(#557),#237,.T.);
#5437=ADVANCED_FACE('',(#558),#238,.T.);
#5438=ADVANCED_FACE('',(#559),#239,.T.);
#5439=ADVANCED_FACE('',(#560),#240,.T.);
#5440=ADVANCED_FACE('',(#561),#5238,.T.);
#5441=ADVANCED_FACE('',(#562),#241,.T.);
#5442=ADVANCED_FACE('',(#563),#242,.T.);
#5443=ADVANCED_FACE('',(#564),#243,.T.);
#5444=ADVANCED_FACE('',(#565),#5239,.T.);
#5445=ADVANCED_FACE('',(#566),#244,.T.);
#5446=ADVANCED_FACE('',(#567),#245,.T.);
#5447=ADVANCED_FACE('',(#568),#246,.T.);
#5448=ADVANCED_FACE('',(#569),#5240,.T.);
#5449=ADVANCED_FACE('',(#570),#5241,.T.);
#5450=ADVANCED_FACE('',(#571),#247,.T.);
#5451=ADVANCED_FACE('',(#572),#248,.T.);
#5452=ADVANCED_FACE('',(#573),#249,.T.);
#5453=ADVANCED_FACE('',(#574),#5242,.T.);
#5454=ADVANCED_FACE('',(#575),#250,.T.);
#5455=ADVANCED_FACE('',(#576),#251,.T.);
#5456=ADVANCED_FACE('',(#577),#252,.T.);
#5457=ADVANCED_FACE('',(#578),#5243,.T.);
#5458=ADVANCED_FACE('',(#579),#253,.T.);
#5459=ADVANCED_FACE('',(#580),#254,.T.);
#5460=ADVANCED_FACE('',(#581),#255,.T.);
#5461=ADVANCED_FACE('',(#582),#256,.T.);
#5462=ADVANCED_FACE('',(#583),#257,.T.);
#5463=ADVANCED_FACE('',(#584),#258,.T.);
#5464=ADVANCED_FACE('',(#585),#5244,.T.);
#5465=ADVANCED_FACE('',(#586),#5245,.T.);
#5466=ADVANCED_FACE('',(#587),#259,.T.);
#5467=ADVANCED_FACE('',(#588),#260,.T.);
#5468=ADVANCED_FACE('',(#589),#261,.T.);
#5469=ADVANCED_FACE('',(#590),#262,.T.);
#5470=ADVANCED_FACE('',(#591),#263,.T.);
#5471=ADVANCED_FACE('',(#592),#264,.T.);
#5472=ADVANCED_FACE('',(#593),#5246,.T.);
#5473=ADVANCED_FACE('',(#594),#5247,.T.);
#5474=ADVANCED_FACE('',(#595),#265,.T.);
#5475=ADVANCED_FACE('',(#596),#266,.T.);
#5476=ADVANCED_FACE('',(#597),#267,.T.);
#5477=ADVANCED_FACE('',(#598),#268,.T.);
#5478=ADVANCED_FACE('',(#599),#269,.T.);
#5479=ADVANCED_FACE('',(#600),#270,.T.);
#5480=ADVANCED_FACE('',(#601),#5248,.T.);
#5481=ADVANCED_FACE('',(#602),#5249,.T.);
#5482=ADVANCED_FACE('',(#603),#271,.T.);
#5483=ADVANCED_FACE('',(#604),#272,.T.);
#5484=ADVANCED_FACE('',(#605),#273,.T.);
#5485=ADVANCED_FACE('',(#606),#5250,.T.);
#5486=ADVANCED_FACE('',(#607),#274,.T.);
#5487=ADVANCED_FACE('',(#608),#275,.T.);
#5488=ADVANCED_FACE('',(#609),#276,.T.);
#5489=ADVANCED_FACE('',(#610),#5251,.T.);
#5490=ADVANCED_FACE('',(#611),#277,.T.);
#5491=ADVANCED_FACE('',(#612),#278,.T.);
#5492=ADVANCED_FACE('',(#613),#279,.T.);
#5493=ADVANCED_FACE('',(#614),#5252,.T.);
#5494=ADVANCED_FACE('',(#615),#280,.T.);
#5495=ADVANCED_FACE('',(#616),#281,.T.);
#5496=ADVANCED_FACE('',(#617),#282,.T.);
#5497=ADVANCED_FACE('',(#618),#5253,.T.);
#5498=ADVANCED_FACE('',(#619),#5254,.T.);
#5499=ADVANCED_FACE('',(#620),#283,.T.);
#5500=ADVANCED_FACE('',(#621),#284,.T.);
#5501=ADVANCED_FACE('',(#622),#285,.T.);
#5502=ADVANCED_FACE('',(#623),#286,.T.);
#5503=ADVANCED_FACE('',(#624),#287,.T.);
#5504=ADVANCED_FACE('',(#625),#288,.T.);
#5505=ADVANCED_FACE('',(#626),#289,.T.);
#5506=ADVANCED_FACE('',(#627),#290,.T.);
#5507=ADVANCED_FACE('',(#628),#291,.T.);
#5508=ADVANCED_FACE('',(#629),#292,.T.);
#5509=ADVANCED_FACE('',(#630),#293,.T.);
#5510=ADVANCED_FACE('',(#631),#5255,.F.);
#5511=ADVANCED_FACE('',(#632),#5256,.F.);
#5512=ADVANCED_FACE('',(#633),#5257,.T.);
#5513=ADVANCED_FACE('',(#634),#5258,.T.);
#5514=ADVANCED_FACE('',(#635),#294,.T.);
#5515=ADVANCED_FACE('',(#636),#295,.T.);
#5516=ADVANCED_FACE('',(#637),#5259,.F.);
#5517=ADVANCED_FACE('',(#638),#5260,.T.);
#5518=ADVANCED_FACE('',(#639),#296,.T.);
#5519=ADVANCED_FACE('',(#640),#297,.T.);
#5520=ADVANCED_FACE('',(#641),#5261,.F.);
#5521=ADVANCED_FACE('',(#642),#5262,.T.);
#5522=ADVANCED_FACE('',(#643),#298,.T.);
#5523=ADVANCED_FACE('',(#644),#299,.T.);
#5524=ADVANCED_FACE('',(#645),#5263,.F.);
#5525=ADVANCED_FACE('',(#646),#5264,.T.);
#5526=ADVANCED_FACE('',(#647),#300,.T.);
#5527=ADVANCED_FACE('',(#648),#301,.T.);
#5528=ADVANCED_FACE('',(#649),#5265,.F.);
#5529=ADVANCED_FACE('',(#650),#5266,.T.);
#5530=ADVANCED_FACE('',(#651),#302,.T.);
#5531=ADVANCED_FACE('',(#652),#303,.T.);
#5532=ADVANCED_FACE('',(#653),#5267,.F.);
#5533=ADVANCED_FACE('',(#654,#126,#127,#128,#129,#130,#131,#132),#304,.T.);
#5534=ADVANCED_FACE('',(#655,#133,#134,#135,#136,#137,#138,#139),#305,.F.);
#5535=ADVANCED_FACE('',(#656),#5268,.F.);
#5536=ADVANCED_FACE('',(#657,#140),#306,.F.);
#5537=ADVANCED_FACE('',(#658,#141),#307,.T.);
#5538=ADVANCED_FACE('',(#659),#308,.T.);
#5539=ADVANCED_FACE('',(#660),#5269,.T.);
#5540=ADVANCED_FACE('',(#661),#309,.T.);
#5541=ADVANCED_FACE('',(#662),#5270,.F.);
#5542=ADVANCED_FACE('',(#663),#310,.T.);
#5543=ADVANCED_FACE('',(#664),#311,.T.);
#5544=ADVANCED_FACE('',(#665,#142),#312,.F.);
#5545=ADVANCED_FACE('',(#666),#313,.F.);
#5546=ADVANCED_FACE('',(#667),#314,.T.);
#5547=ADVANCED_FACE('',(#668),#5271,.F.);
#5548=ADVANCED_FACE('',(#669),#5272,.T.);
#5549=ADVANCED_FACE('',(#670),#315,.T.);
#5550=ADVANCED_FACE('',(#671),#5273,.T.);
#5551=ADVANCED_FACE('',(#672),#316,.T.);
#5552=ADVANCED_FACE('',(#673),#5274,.F.);
#5553=ADVANCED_FACE('',(#674),#317,.T.);
#5554=ADVANCED_FACE('',(#675),#5275,.T.);
#5555=ADVANCED_FACE('',(#676),#318,.T.);
#5556=ADVANCED_FACE('',(#677),#5276,.F.);
#5557=ADVANCED_FACE('',(#678),#5277,.F.);
#5558=ADVANCED_FACE('',(#679),#5278,.F.);
#5559=ADVANCED_FACE('',(#680),#395,.F.);
#5560=ADVANCED_FACE('',(#681),#360,.T.);
#5561=ADVANCED_FACE('',(#682),#5279,.T.);
#5562=ADVANCED_FACE('',(#683),#361,.T.);
#5563=ADVANCED_FACE('',(#684),#396,.F.);
#5564=ADVANCED_FACE('',(#685,#143),#319,.F.);
#5565=ADVANCED_FACE('',(#686,#144),#320,.F.);
#5566=ADVANCED_FACE('',(#687,#145),#321,.F.);
#5567=ADVANCED_FACE('',(#688,#146),#322,.F.);
#5568=ADVANCED_FACE('',(#689),#397,.T.);
#5569=ADVANCED_FACE('',(#690),#5280,.T.);
#5570=ADVANCED_FACE('',(#691),#362,.F.);
#5571=ADVANCED_FACE('',(#692),#5281,.T.);
#5572=ADVANCED_FACE('',(#693),#363,.F.);
#5573=ADVANCED_FACE('',(#694),#5282,.T.);
#5574=ADVANCED_FACE('',(#695),#398,.T.);
#5575=ADVANCED_FACE('',(#696),#364,.T.);
#5576=ADVANCED_FACE('',(#697),#5283,.F.);
#5577=ADVANCED_FACE('',(#698),#365,.T.);
#5578=ADVANCED_FACE('',(#699,#147),#323,.F.);
#5579=ADVANCED_FACE('',(#700,#148),#324,.F.);
#5580=ADVANCED_FACE('',(#701,#149),#325,.F.);
#5581=ADVANCED_FACE('',(#702,#150),#326,.F.);
#5582=ADVANCED_FACE('',(#703),#5284,.F.);
#5583=ADVANCED_FACE('',(#704),#366,.T.);
#5584=ADVANCED_FACE('',(#705),#399,.T.);
#5585=ADVANCED_FACE('',(#706),#367,.F.);
#5586=ADVANCED_FACE('',(#707),#368,.F.);
#5587=ADVANCED_FACE('',(#708),#400,.F.);
#5588=ADVANCED_FACE('',(#709),#369,.F.);
#5589=ADVANCED_FACE('',(#710),#370,.T.);
#5590=ADVANCED_FACE('',(#711),#401,.T.);
#5591=ADVANCED_FACE('',(#712),#371,.T.);
#5592=ADVANCED_FACE('',(#713),#372,.T.);
#5593=ADVANCED_FACE('',(#714),#402,.F.);
#5594=ADVANCED_FACE('',(#715,#151),#327,.F.);
#5595=ADVANCED_FACE('',(#716,#152),#328,.F.);
#5596=ADVANCED_FACE('',(#717,#153),#329,.T.);
#5597=ADVANCED_FACE('',(#718,#154),#330,.T.);
#5598=ADVANCED_FACE('',(#719,#155),#331,.T.);
#5599=ADVANCED_FACE('',(#720),#5285,.F.);
#5600=ADVANCED_FACE('',(#721),#373,.T.);
#5601=ADVANCED_FACE('',(#722),#403,.T.);
#5602=ADVANCED_FACE('',(#723),#374,.F.);
#5603=ADVANCED_FACE('',(#724),#375,.F.);
#5604=ADVANCED_FACE('',(#725),#404,.F.);
#5605=ADVANCED_FACE('',(#726),#376,.F.);
#5606=ADVANCED_FACE('',(#727),#377,.T.);
#5607=ADVANCED_FACE('',(#728),#405,.T.);
#5608=ADVANCED_FACE('',(#729),#378,.T.);
#5609=ADVANCED_FACE('',(#730),#379,.T.);
#5610=ADVANCED_FACE('',(#731),#406,.F.);
#5611=ADVANCED_FACE('',(#732,#156),#332,.F.);
#5612=ADVANCED_FACE('',(#733,#157),#333,.F.);
#5613=ADVANCED_FACE('',(#734,#158),#334,.T.);
#5614=ADVANCED_FACE('',(#735,#159),#335,.T.);
#5615=ADVANCED_FACE('',(#736,#160),#336,.T.);
#5616=CLOSED_SHELL('',(#5286,#5287,#5288,#5289,#5290,#5291,#5292,#5293,
#5294,#5295,#5296,#5297));
#5617=CLOSED_SHELL('',(#5298,#5299,#5300,#5301,#5302,#5303,#5304,#5305,
#5306,#5307,#5308,#5309,#5310,#5311));
#5618=CLOSED_SHELL('',(#5312,#5313,#5314,#5315,#5316,#5317,#5318,#5319,
#5320,#5321,#5322,#5323,#5324,#5325,#5326,#5327,#5328));
#5619=CLOSED_SHELL('',(#5329,#5330,#5331,#5332,#5333,#5334,#5335,#5336,
#5337,#5338,#5339,#5340,#5341,#5342,#5343,#5344,#5345));
#5620=CLOSED_SHELL('',(#5346,#5347,#5348,#5349,#5350,#5351,#5352,#5353,
#5354,#5355,#5356,#5357,#5358));
#5621=CLOSED_SHELL('',(#5359,#5360,#5361,#5362,#5363,#5364,#5365,#5366,
#5367,#5368,#5369,#5370,#5371,#5372,#5373,#5374));
#5622=CLOSED_SHELL('',(#5375,#5376,#5377,#5378));
#5623=CLOSED_SHELL('',(#5379,#5380,#5381,#5382,#5383,#5384,#5385,#5386,
#5387));
#5624=CLOSED_SHELL('',(#5388,#5389,#5390,#5391,#5392,#5393,#5394,#5395,
#5396,#5397,#5398,#5399,#5400,#5401,#5402,#5403,#5404,#5405,#5406,#5407,
#5408,#5409,#5410,#5411,#5412,#5413,#5414,#5415,#5416,#5417,#5418,#5419,
#5420,#5421,#5422,#5423,#5424,#5425,#5426,#5427,#5428,#5429,#5430,#5431,
#5432,#5433,#5434,#5435,#5436,#5437,#5438,#5439,#5440,#5441,#5442,#5443,
#5444,#5445,#5446,#5447,#5448,#5449,#5450,#5451,#5452,#5453,#5454,#5455,
#5456,#5457,#5458,#5459,#5460,#5461,#5462,#5463,#5464,#5465,#5466,#5467,
#5468,#5469,#5470,#5471,#5472,#5473,#5474,#5475,#5476,#5477,#5478,#5479,
#5480,#5481,#5482,#5483,#5484,#5485,#5486,#5487,#5488,#5489,#5490,#5491,
#5492,#5493,#5494,#5495,#5496,#5497,#5498,#5499,#5500,#5501,#5502,#5503,
#5504,#5505,#5506,#5507,#5508,#5509,#5510,#5511,#5512,#5513,#5514,#5515,
#5516,#5517,#5518,#5519,#5520,#5521,#5522,#5523,#5524,#5525,#5526,#5527,
#5528,#5529,#5530,#5531,#5532,#5533,#5534));
#5625=CLOSED_SHELL('',(#5535,#5536,#5537,#5538,#5539,#5540,#5541,#5542,
#5543,#5544,#5545,#5546,#5547,#5548,#5549,#5550,#5551,#5552,#5553,#5554,
#5555));
#5626=CLOSED_SHELL('',(#5556,#5557,#5558,#5559,#5560,#5561,#5562,#5563,
#5564,#5565,#5566,#5567));
#5627=CLOSED_SHELL('',(#5568,#5569,#5570,#5571,#5572,#5573,#5574,#5575,
#5576,#5577,#5578,#5579,#5580,#5581));
#5628=CLOSED_SHELL('',(#5582,#5583,#5584,#5585,#5586,#5587,#5588,#5589,
#5590,#5591,#5592,#5593,#5594,#5595,#5596,#5597,#5598));
#5629=CLOSED_SHELL('',(#5599,#5600,#5601,#5602,#5603,#5604,#5605,#5606,
#5607,#5608,#5609,#5610,#5611,#5612,#5613,#5614,#5615));
#5630=DERIVED_UNIT_ELEMENT(#5646,1.);
#5631=DERIVED_UNIT_ELEMENT(#9893,-3.);
#5632=DERIVED_UNIT_ELEMENT(#5646,1.);
#5633=DERIVED_UNIT_ELEMENT(#9893,-3.);
#5634=DERIVED_UNIT_ELEMENT(#5646,1.);
#5635=DERIVED_UNIT_ELEMENT(#9893,-3.);
#5636=DERIVED_UNIT_ELEMENT(#5646,1.);
#5637=DERIVED_UNIT_ELEMENT(#9893,-3.);
#5638=DERIVED_UNIT_ELEMENT(#5646,1.);
#5639=DERIVED_UNIT_ELEMENT(#9893,-3.);
#5640=DERIVED_UNIT_ELEMENT(#5646,1.);
#5641=DERIVED_UNIT_ELEMENT(#9893,-3.);
#5642=DERIVED_UNIT_ELEMENT(#5646,1.);
#5643=DERIVED_UNIT_ELEMENT(#9893,-3.);
#5644=DERIVED_UNIT_ELEMENT(#5646,1.);
#5645=DERIVED_UNIT_ELEMENT(#9893,-3.);
#5646=(
MASS_UNIT()
NAMED_UNIT(*)
SI_UNIT(.KILO.,.GRAM.)
);
#5647=DERIVED_UNIT((#5630,#5631));
#5648=DERIVED_UNIT((#5632,#5633));
#5649=DERIVED_UNIT((#5634,#5635));
#5650=DERIVED_UNIT((#5636,#5637));
#5651=DERIVED_UNIT((#5638,#5639));
#5652=DERIVED_UNIT((#5640,#5641));
#5653=DERIVED_UNIT((#5642,#5643));
#5654=DERIVED_UNIT((#5644,#5645));
#5655=MEASURE_REPRESENTATION_ITEM('density measure',
POSITIVE_RATIO_MEASURE(7850.),#5647);
#5656=MEASURE_REPRESENTATION_ITEM('density measure',
POSITIVE_RATIO_MEASURE(7750.),#5648);
#5657=MEASURE_REPRESENTATION_ITEM('density measure',
POSITIVE_RATIO_MEASURE(7850.),#5649);
#5658=MEASURE_REPRESENTATION_ITEM('density measure',
POSITIVE_RATIO_MEASURE(7850.),#5650);
#5659=MEASURE_REPRESENTATION_ITEM('density measure',
POSITIVE_RATIO_MEASURE(7850.),#5651);
#5660=MEASURE_REPRESENTATION_ITEM('density measure',
POSITIVE_RATIO_MEASURE(7850.),#5652);
#5661=MEASURE_REPRESENTATION_ITEM('density measure',
POSITIVE_RATIO_MEASURE(7850.),#5653);
#5662=MEASURE_REPRESENTATION_ITEM('density measure',
POSITIVE_RATIO_MEASURE(7850.),#5654);
#5663=PROPERTY_DEFINITION_REPRESENTATION(#5703,#5679);
#5664=PROPERTY_DEFINITION_REPRESENTATION(#5704,#5680);
#5665=PROPERTY_DEFINITION_REPRESENTATION(#5705,#5681);
#5666=PROPERTY_DEFINITION_REPRESENTATION(#5706,#5682);
#5667=PROPERTY_DEFINITION_REPRESENTATION(#5707,#5683);
#5668=PROPERTY_DEFINITION_REPRESENTATION(#5708,#5684);
#5669=PROPERTY_DEFINITION_REPRESENTATION(#5709,#5685);
#5670=PROPERTY_DEFINITION_REPRESENTATION(#5710,#5686);
#5671=PROPERTY_DEFINITION_REPRESENTATION(#5711,#5687);
#5672=PROPERTY_DEFINITION_REPRESENTATION(#5712,#5688);
#5673=PROPERTY_DEFINITION_REPRESENTATION(#5713,#5689);
#5674=PROPERTY_DEFINITION_REPRESENTATION(#5714,#5690);
#5675=PROPERTY_DEFINITION_REPRESENTATION(#5715,#5691);
#5676=PROPERTY_DEFINITION_REPRESENTATION(#5716,#5692);
#5677=PROPERTY_DEFINITION_REPRESENTATION(#5717,#5693);
#5678=PROPERTY_DEFINITION_REPRESENTATION(#5718,#5694);
#5679=REPRESENTATION('material name',(#5695),#9883);
#5680=REPRESENTATION('density',(#5655),#9883);
#5681=REPRESENTATION('material name',(#5696),#9884);
#5682=REPRESENTATION('density',(#5656),#9884);
#5683=REPRESENTATION('material name',(#5697),#9885);
#5684=REPRESENTATION('density',(#5657),#9885);
#5685=REPRESENTATION('material name',(#5698),#9886);
#5686=REPRESENTATION('density',(#5658),#9886);
#5687=REPRESENTATION('material name',(#5699),#9887);
#5688=REPRESENTATION('density',(#5659),#9887);
#5689=REPRESENTATION('material name',(#5700),#9888);
#5690=REPRESENTATION('density',(#5660),#9888);
#5691=REPRESENTATION('material name',(#5701),#9889);
#5692=REPRESENTATION('density',(#5661),#9889);
#5693=REPRESENTATION('material name',(#5702),#9890);
#5694=REPRESENTATION('density',(#5662),#9890);
#5695=DESCRIPTIVE_REPRESENTATION_ITEM('Steel','Steel');
#5696=DESCRIPTIVE_REPRESENTATION_ITEM('Steel 4.6, Plain',
'Steel 4.6, Plain');
#5697=DESCRIPTIVE_REPRESENTATION_ITEM('Steel','Steel');
#5698=DESCRIPTIVE_REPRESENTATION_ITEM('Steel','Steel');
#5699=DESCRIPTIVE_REPRESENTATION_ITEM('Steel','Steel');
#5700=DESCRIPTIVE_REPRESENTATION_ITEM('Steel','Steel');
#5701=DESCRIPTIVE_REPRESENTATION_ITEM('Steel','Steel');
#5702=DESCRIPTIVE_REPRESENTATION_ITEM('Steel','Steel');
#5703=PROPERTY_DEFINITION('material property','material name',#9933);
#5704=PROPERTY_DEFINITION('material property','density of part',#9933);
#5705=PROPERTY_DEFINITION('material property','material name',#9934);
#5706=PROPERTY_DEFINITION('material property','density of part',#9934);
#5707=PROPERTY_DEFINITION('material property','material name',#9935);
#5708=PROPERTY_DEFINITION('material property','density of part',#9935);
#5709=PROPERTY_DEFINITION('material property','material name',#9936);
#5710=PROPERTY_DEFINITION('material property','density of part',#9936);
#5711=PROPERTY_DEFINITION('material property','material name',#9937);
#5712=PROPERTY_DEFINITION('material property','density of part',#9937);
#5713=PROPERTY_DEFINITION('material property','material name',#9938);
#5714=PROPERTY_DEFINITION('material property','density of part',#9938);
#5715=PROPERTY_DEFINITION('material property','material name',#9939);
#5716=PROPERTY_DEFINITION('material property','density of part',#9939);
#5717=PROPERTY_DEFINITION('material property','material name',#9940);
#5718=PROPERTY_DEFINITION('material property','density of part',#9940);
#5719=AXIS2_PLACEMENT_3D('',#8139,#6371,#6372);
#5720=AXIS2_PLACEMENT_3D('',#8140,#6373,#6374);
#5721=AXIS2_PLACEMENT_3D('',#8141,#6375,#6376);
#5722=AXIS2_PLACEMENT_3D('',#8143,#6377,#6378);
#5723=AXIS2_PLACEMENT_3D('',#8146,#6380,#6381);
#5724=AXIS2_PLACEMENT_3D('',#8147,#6382,#6383);
#5725=AXIS2_PLACEMENT_3D('',#8149,#6384,#6385);
#5726=AXIS2_PLACEMENT_3D('',#8152,#6387,#6388);
#5727=AXIS2_PLACEMENT_3D('',#8153,#6389,#6390);
#5728=AXIS2_PLACEMENT_3D('',#8156,#6391,#6392);
#5729=AXIS2_PLACEMENT_3D('',#8157,#6393,#6394);
#5730=AXIS2_PLACEMENT_3D('',#8160,#6396,#6397);
#5731=AXIS2_PLACEMENT_3D('',#8161,#6398,#6399);
#5732=AXIS2_PLACEMENT_3D('',#8164,#6401,#6402);
#5733=AXIS2_PLACEMENT_3D('',#8165,#6403,#6404);
#5734=AXIS2_PLACEMENT_3D('',#8167,#6405,#6406);
#5735=AXIS2_PLACEMENT_3D('',#8169,#6407,#6408);
#5736=AXIS2_PLACEMENT_3D('',#8170,#6409,#6410);
#5737=AXIS2_PLACEMENT_3D('',#8171,#6411,#6412);
#5738=AXIS2_PLACEMENT_3D('',#8173,#6413,#6414);
#5739=AXIS2_PLACEMENT_3D('',#8175,#6416,#6417);
#5740=AXIS2_PLACEMENT_3D('',#8177,#6418,#6419);
#5741=AXIS2_PLACEMENT_3D('',#8178,#6420,#6421);
#5742=AXIS2_PLACEMENT_3D('',#8179,#6422,#6423);
#5743=AXIS2_PLACEMENT_3D('',#8182,#6425,#6426);
#5744=AXIS2_PLACEMENT_3D('',#8183,#6427,#6428);
#5745=AXIS2_PLACEMENT_3D('',#8184,#6429,#6430);
#5746=AXIS2_PLACEMENT_3D('',#8185,#6431,#6432);
#5747=AXIS2_PLACEMENT_3D('',#8186,#6433,#6434);
#5748=AXIS2_PLACEMENT_3D('',#8187,#6435,#6436);
#5749=AXIS2_PLACEMENT_3D('',#8190,#6437,#6438);
#5750=AXIS2_PLACEMENT_3D('',#8193,#6440,#6441);
#5751=AXIS2_PLACEMENT_3D('',#8194,#6442,#6443);
#5752=AXIS2_PLACEMENT_3D('',#8195,#6444,#6445);
#5753=AXIS2_PLACEMENT_3D('',#8198,#6447,#6448);
#5754=AXIS2_PLACEMENT_3D('',#8199,#6449,#6450);
#5755=AXIS2_PLACEMENT_3D('',#8201,#6451,#6452);
#5756=AXIS2_PLACEMENT_3D('',#8202,#6453,#6454);
#5757=AXIS2_PLACEMENT_3D('',#8203,#6455,#6456);
#5758=AXIS2_PLACEMENT_3D('',#8205,#6457,#6458);
#5759=AXIS2_PLACEMENT_3D('',#8208,#6460,#6461);
#5760=AXIS2_PLACEMENT_3D('',#8209,#6462,#6463);
#5761=AXIS2_PLACEMENT_3D('',#8211,#6464,#6465);
#5762=AXIS2_PLACEMENT_3D('',#8213,#6466,#6467);
#5763=AXIS2_PLACEMENT_3D('',#8214,#6468,#6469);
#5764=AXIS2_PLACEMENT_3D('',#8215,#6470,#6471);
#5765=AXIS2_PLACEMENT_3D('',#8218,#6473,#6474);
#5766=AXIS2_PLACEMENT_3D('',#8219,#6475,#6476);
#5767=AXIS2_PLACEMENT_3D('',#8222,#6478,#6479);
#5768=AXIS2_PLACEMENT_3D('',#8223,#6480,#6481);
#5769=AXIS2_PLACEMENT_3D('',#8225,#6482,#6483);
#5770=AXIS2_PLACEMENT_3D('',#8227,#6484,#6485);
#5771=AXIS2_PLACEMENT_3D('',#8228,#6486,#6487);
#5772=AXIS2_PLACEMENT_3D('',#8229,#6488,#6489);
#5773=AXIS2_PLACEMENT_3D('',#8232,#6491,#6492);
#5774=AXIS2_PLACEMENT_3D('',#8233,#6493,#6494);
#5775=AXIS2_PLACEMENT_3D('',#8235,#6495,#6496);
#5776=AXIS2_PLACEMENT_3D('',#8236,#6497,#6498);
#5777=AXIS2_PLACEMENT_3D('',#8237,#6499,#6500);
#5778=AXIS2_PLACEMENT_3D('',#8238,#6501,#6502);
#5779=AXIS2_PLACEMENT_3D('',#8239,#6503,#6504);
#5780=AXIS2_PLACEMENT_3D('',#8240,#6505,#6506);
#5781=AXIS2_PLACEMENT_3D('',#8241,#6507,#6508);
#5782=AXIS2_PLACEMENT_3D('',#8243,#6509,#6510);
#5783=AXIS2_PLACEMENT_3D('',#8246,#6512,#6513);
#5784=AXIS2_PLACEMENT_3D('',#8247,#6514,#6515);
#5785=AXIS2_PLACEMENT_3D('',#8249,#6516,#6517);
#5786=AXIS2_PLACEMENT_3D('',#8251,#6518,#6519);
#5787=AXIS2_PLACEMENT_3D('',#8252,#6520,#6521);
#5788=AXIS2_PLACEMENT_3D('',#8253,#6522,#6523);
#5789=AXIS2_PLACEMENT_3D('',#8255,#6524,#6525);
#5790=AXIS2_PLACEMENT_3D('',#8257,#6527,#6528);
#5791=AXIS2_PLACEMENT_3D('',#8259,#6529,#6530);
#5792=AXIS2_PLACEMENT_3D('',#8260,#6531,#6532);
#5793=AXIS2_PLACEMENT_3D('',#8261,#6533,#6534);
#5794=AXIS2_PLACEMENT_3D('',#8263,#6535,#6536);
#5795=AXIS2_PLACEMENT_3D('',#8265,#6537,#6538);
#5796=AXIS2_PLACEMENT_3D('',#8266,#6539,#6540);
#5797=AXIS2_PLACEMENT_3D('',#8267,#6541,#6542);
#5798=AXIS2_PLACEMENT_3D('',#8269,#6543,#6544);
#5799=AXIS2_PLACEMENT_3D('',#8271,#6546,#6547);
#5800=AXIS2_PLACEMENT_3D('',#8273,#6548,#6549);
#5801=AXIS2_PLACEMENT_3D('',#8274,#6550,#6551);
#5802=AXIS2_PLACEMENT_3D('',#8275,#6552,#6553);
#5803=AXIS2_PLACEMENT_3D('',#8277,#6554,#6555);
#5804=AXIS2_PLACEMENT_3D('',#8279,#6556,#6557);
#5805=AXIS2_PLACEMENT_3D('',#8280,#6558,#6559);
#5806=AXIS2_PLACEMENT_3D('',#8281,#6560,#6561);
#5807=AXIS2_PLACEMENT_3D('',#8283,#6562,#6563);
#5808=AXIS2_PLACEMENT_3D('',#8285,#6565,#6566);
#5809=AXIS2_PLACEMENT_3D('',#8287,#6567,#6568);
#5810=AXIS2_PLACEMENT_3D('',#8288,#6569,#6570);
#5811=AXIS2_PLACEMENT_3D('',#8289,#6571,#6572);
#5812=AXIS2_PLACEMENT_3D('',#8291,#6573,#6574);
#5813=AXIS2_PLACEMENT_3D('',#8293,#6575,#6576);
#5814=AXIS2_PLACEMENT_3D('',#8294,#6577,#6578);
#5815=AXIS2_PLACEMENT_3D('',#8295,#6579,#6580);
#5816=AXIS2_PLACEMENT_3D('',#8297,#6581,#6582);
#5817=AXIS2_PLACEMENT_3D('',#8299,#6584,#6585);
#5818=AXIS2_PLACEMENT_3D('',#8300,#6586,#6587);
#5819=AXIS2_PLACEMENT_3D('',#8301,#6588,#6589);
#5820=AXIS2_PLACEMENT_3D('',#8302,#6590,#6591);
#5821=AXIS2_PLACEMENT_3D('',#8303,#6592,#6593);
#5822=AXIS2_PLACEMENT_3D('',#8304,#6594,#6595);
#5823=AXIS2_PLACEMENT_3D('',#8306,#6596,#6597);
#5824=AXIS2_PLACEMENT_3D('',#8309,#6599,#6600);
#5825=AXIS2_PLACEMENT_3D('',#8310,#6601,#6602);
#5826=AXIS2_PLACEMENT_3D('',#8312,#6603,#6604);
#5827=AXIS2_PLACEMENT_3D('',#8314,#6605,#6606);
#5828=AXIS2_PLACEMENT_3D('',#8315,#6607,#6608);
#5829=AXIS2_PLACEMENT_3D('',#8316,#6609,#6610);
#5830=AXIS2_PLACEMENT_3D('',#8318,#6611,#6612);
#5831=AXIS2_PLACEMENT_3D('',#8320,#6614,#6615);
#5832=AXIS2_PLACEMENT_3D('',#8322,#6616,#6617);
#5833=AXIS2_PLACEMENT_3D('',#8323,#6618,#6619);
#5834=AXIS2_PLACEMENT_3D('',#8324,#6620,#6621);
#5835=AXIS2_PLACEMENT_3D('',#8326,#6622,#6623);
#5836=AXIS2_PLACEMENT_3D('',#8328,#6624,#6625);
#5837=AXIS2_PLACEMENT_3D('',#8329,#6626,#6627);
#5838=AXIS2_PLACEMENT_3D('',#8330,#6628,#6629);
#5839=AXIS2_PLACEMENT_3D('',#8332,#6630,#6631);
#5840=AXIS2_PLACEMENT_3D('',#8334,#6633,#6634);
#5841=AXIS2_PLACEMENT_3D('',#8336,#6635,#6636);
#5842=AXIS2_PLACEMENT_3D('',#8337,#6637,#6638);
#5843=AXIS2_PLACEMENT_3D('',#8338,#6639,#6640);
#5844=AXIS2_PLACEMENT_3D('',#8340,#6641,#6642);
#5845=AXIS2_PLACEMENT_3D('',#8342,#6643,#6644);
#5846=AXIS2_PLACEMENT_3D('',#8343,#6645,#6646);
#5847=AXIS2_PLACEMENT_3D('',#8344,#6647,#6648);
#5848=AXIS2_PLACEMENT_3D('',#8346,#6649,#6650);
#5849=AXIS2_PLACEMENT_3D('',#8348,#6652,#6653);
#5850=AXIS2_PLACEMENT_3D('',#8350,#6654,#6655);
#5851=AXIS2_PLACEMENT_3D('',#8351,#6656,#6657);
#5852=AXIS2_PLACEMENT_3D('',#8352,#6658,#6659);
#5853=AXIS2_PLACEMENT_3D('',#8354,#6660,#6661);
#5854=AXIS2_PLACEMENT_3D('',#8356,#6662,#6663);
#5855=AXIS2_PLACEMENT_3D('',#8357,#6664,#6665);
#5856=AXIS2_PLACEMENT_3D('',#8358,#6666,#6667);
#5857=AXIS2_PLACEMENT_3D('',#8360,#6668,#6669);
#5858=AXIS2_PLACEMENT_3D('',#8362,#6671,#6672);
#5859=AXIS2_PLACEMENT_3D('',#8363,#6673,#6674);
#5860=AXIS2_PLACEMENT_3D('',#8364,#6675,#6676);
#5861=AXIS2_PLACEMENT_3D('',#8365,#6677,#6678);
#5862=AXIS2_PLACEMENT_3D('',#8366,#6679,#6680);
#5863=AXIS2_PLACEMENT_3D('',#8367,#6681,#6682);
#5864=AXIS2_PLACEMENT_3D('',#8368,#6683,#6684);
#5865=AXIS2_PLACEMENT_3D('',#8370,#6685,#6686);
#5866=AXIS2_PLACEMENT_3D('',#8373,#6688,#6689);
#5867=AXIS2_PLACEMENT_3D('',#8374,#6690,#6691);
#5868=AXIS2_PLACEMENT_3D('',#8401,#6694,#6695);
#5869=AXIS2_PLACEMENT_3D('',#8428,#6698,#6699);
#5870=AXIS2_PLACEMENT_3D('',#8429,#6700,#6701);
#5871=AXIS2_PLACEMENT_3D('',#8431,#6702,#6703);
#5872=AXIS2_PLACEMENT_3D('',#8432,#6704,#6705);
#5873=AXIS2_PLACEMENT_3D('',#8433,#6706,#6707);
#5874=AXIS2_PLACEMENT_3D('',#8434,#6708,#6709);
#5875=AXIS2_PLACEMENT_3D('',#8435,#6710,#6711);
#5876=AXIS2_PLACEMENT_3D('',#8436,#6712,#6713);
#5877=AXIS2_PLACEMENT_3D('',#8437,#6714,#6715);
#5878=AXIS2_PLACEMENT_3D('',#8439,#6716,#6717);
#5879=AXIS2_PLACEMENT_3D('',#8440,#6718,#6719);
#5880=AXIS2_PLACEMENT_3D('',#8441,#6720,#6721);
#5881=AXIS2_PLACEMENT_3D('',#8443,#6722,#6723);
#5882=AXIS2_PLACEMENT_3D('',#8445,#6725,#6726);
#5883=AXIS2_PLACEMENT_3D('',#8446,#6727,#6728);
#5884=AXIS2_PLACEMENT_3D('',#8448,#6729,#6730);
#5885=AXIS2_PLACEMENT_3D('',#8449,#6731,#6732);
#5886=AXIS2_PLACEMENT_3D('',#8451,#6733,#6734);
#5887=AXIS2_PLACEMENT_3D('',#8453,#6736,#6737);
#5888=AXIS2_PLACEMENT_3D('',#8455,#6738,#6739);
#5889=AXIS2_PLACEMENT_3D('',#8457,#6741,#6742);
#5890=AXIS2_PLACEMENT_3D('',#8459,#6744,#6745);
#5891=AXIS2_PLACEMENT_3D('',#8460,#6746,#6747);
#5892=AXIS2_PLACEMENT_3D('',#8462,#6748,#6749);
#5893=AXIS2_PLACEMENT_3D('',#8465,#6751,#6752);
#5894=AXIS2_PLACEMENT_3D('',#8466,#6753,#6754);
#5895=AXIS2_PLACEMENT_3D('',#8468,#6755,#6756);
#5896=AXIS2_PLACEMENT_3D('',#8471,#6758,#6759);
#5897=AXIS2_PLACEMENT_3D('',#8472,#6760,#6761);
#5898=AXIS2_PLACEMENT_3D('',#8474,#6762,#6763);
#5899=AXIS2_PLACEMENT_3D('',#8477,#6765,#6766);
#5900=AXIS2_PLACEMENT_3D('',#8478,#6767,#6768);
#5901=AXIS2_PLACEMENT_3D('',#8480,#6769,#6770);
#5902=AXIS2_PLACEMENT_3D('',#8483,#6772,#6773);
#5903=AXIS2_PLACEMENT_3D('',#8484,#6774,#6775);
#5904=AXIS2_PLACEMENT_3D('',#8485,#6776,#6777);
#5905=AXIS2_PLACEMENT_3D('',#8495,#6782,#6783);
#5906=AXIS2_PLACEMENT_3D('',#8496,#6784,#6785);
#5907=AXIS2_PLACEMENT_3D('',#8498,#6786,#6787);
#5908=AXIS2_PLACEMENT_3D('',#8501,#6789,#6790);
#5909=AXIS2_PLACEMENT_3D('',#8502,#6791,#6792);
#5910=AXIS2_PLACEMENT_3D('',#8504,#6793,#6794);
#5911=AXIS2_PLACEMENT_3D('',#8506,#6796,#6797);
#5912=AXIS2_PLACEMENT_3D('',#8507,#6798,#6799);
#5913=AXIS2_PLACEMENT_3D('',#8508,#6800,#6801);
#5914=AXIS2_PLACEMENT_3D('',#8514,#6805,#6806);
#5915=AXIS2_PLACEMENT_3D('',#8518,#6809,#6810);
#5916=AXIS2_PLACEMENT_3D('',#8522,#6813,#6814);
#5917=AXIS2_PLACEMENT_3D('',#8524,#6816,#6817);
#5918=AXIS2_PLACEMENT_3D('',#8525,#6818,#6819);
#5919=AXIS2_PLACEMENT_3D('',#8526,#6820,#6821);
#5920=AXIS2_PLACEMENT_3D('',#8527,#6822,#6823);
#5921=AXIS2_PLACEMENT_3D('',#8529,#6824,#6825);
#5922=AXIS2_PLACEMENT_3D('',#8532,#6827,#6828);
#5923=AXIS2_PLACEMENT_3D('',#8533,#6829,#6830);
#5924=AXIS2_PLACEMENT_3D('',#8535,#6831,#6832);
#5925=AXIS2_PLACEMENT_3D('',#8538,#6834,#6835);
#5926=AXIS2_PLACEMENT_3D('',#8539,#6836,#6837);
#5927=AXIS2_PLACEMENT_3D('',#8540,#6838,#6839);
#5928=AXIS2_PLACEMENT_3D('',#8541,#6840,#6841);
#5929=AXIS2_PLACEMENT_3D('',#8542,#6842,#6843);
#5930=AXIS2_PLACEMENT_3D('',#8544,#6844,#6845);
#5931=AXIS2_PLACEMENT_3D('',#8546,#6846,#6847);
#5932=AXIS2_PLACEMENT_3D('',#8548,#6848,#6849);
#5933=AXIS2_PLACEMENT_3D('',#8549,#6850,#6851);
#5934=AXIS2_PLACEMENT_3D('',#8550,#6852,#6853);
#5935=AXIS2_PLACEMENT_3D('',#8590,#6855,#6856);
#5936=AXIS2_PLACEMENT_3D('',#8591,#6857,#6858);
#5937=AXIS2_PLACEMENT_3D('',#8593,#6859,#6860);
#5938=AXIS2_PLACEMENT_3D('',#8595,#6861,#6862);
#5939=AXIS2_PLACEMENT_3D('',#8597,#6863,#6864);
#5940=AXIS2_PLACEMENT_3D('',#8598,#6865,#6866);
#5941=AXIS2_PLACEMENT_3D('',#8599,#6867,#6868);
#5942=AXIS2_PLACEMENT_3D('',#8642,#6870,#6871);
#5943=AXIS2_PLACEMENT_3D('',#8643,#6872,#6873);
#5944=AXIS2_PLACEMENT_3D('',#8645,#6874,#6875);
#5945=AXIS2_PLACEMENT_3D('',#8646,#6876,#6877);
#5946=AXIS2_PLACEMENT_3D('',#8648,#6878,#6879);
#5947=AXIS2_PLACEMENT_3D('',#8651,#6882,#6883);
#5948=AXIS2_PLACEMENT_3D('',#8652,#6884,#6885);
#5949=AXIS2_PLACEMENT_3D('',#8653,#6886,#6887);
#5950=AXIS2_PLACEMENT_3D('',#8662,#6892,#6893);
#5951=AXIS2_PLACEMENT_3D('',#8668,#6897,#6898);
#5952=AXIS2_PLACEMENT_3D('',#8674,#6902,#6903);
#5953=AXIS2_PLACEMENT_3D('',#8676,#6904,#6905);
#5954=AXIS2_PLACEMENT_3D('',#8679,#6907,#6908);
#5955=AXIS2_PLACEMENT_3D('',#8680,#6909,#6910);
#5956=AXIS2_PLACEMENT_3D('',#8682,#6911,#6912);
#5957=AXIS2_PLACEMENT_3D('',#8685,#6914,#6915);
#5958=AXIS2_PLACEMENT_3D('',#8686,#6916,#6917);
#5959=AXIS2_PLACEMENT_3D('',#8695,#6922,#6923);
#5960=AXIS2_PLACEMENT_3D('',#8701,#6927,#6928);
#5961=AXIS2_PLACEMENT_3D('',#8704,#6931,#6932);
#5962=AXIS2_PLACEMENT_3D('',#8706,#6933,#6934);
#5963=AXIS2_PLACEMENT_3D('',#8709,#6936,#6937);
#5964=AXIS2_PLACEMENT_3D('',#8710,#6938,#6939);
#5965=AXIS2_PLACEMENT_3D('',#8719,#6944,#6945);
#5966=AXIS2_PLACEMENT_3D('',#8725,#6949,#6950);
#5967=AXIS2_PLACEMENT_3D('',#8728,#6953,#6954);
#5968=AXIS2_PLACEMENT_3D('',#8730,#6955,#6956);
#5969=AXIS2_PLACEMENT_3D('',#8733,#6958,#6959);
#5970=AXIS2_PLACEMENT_3D('',#8734,#6960,#6961);
#5971=AXIS2_PLACEMENT_3D('',#8743,#6966,#6967);
#5972=AXIS2_PLACEMENT_3D('',#8749,#6971,#6972);
#5973=AXIS2_PLACEMENT_3D('',#8752,#6975,#6976);
#5974=AXIS2_PLACEMENT_3D('',#8754,#6977,#6978);
#5975=AXIS2_PLACEMENT_3D('',#8757,#6980,#6981);
#5976=AXIS2_PLACEMENT_3D('',#8758,#6982,#6983);
#5977=AXIS2_PLACEMENT_3D('',#8767,#6988,#6989);
#5978=AXIS2_PLACEMENT_3D('',#8773,#6993,#6994);
#5979=AXIS2_PLACEMENT_3D('',#8776,#6997,#6998);
#5980=AXIS2_PLACEMENT_3D('',#8778,#6999,#7000);
#5981=AXIS2_PLACEMENT_3D('',#8781,#7002,#7003);
#5982=AXIS2_PLACEMENT_3D('',#8782,#7004,#7005);
#5983=AXIS2_PLACEMENT_3D('',#8791,#7010,#7011);
#5984=AXIS2_PLACEMENT_3D('',#8797,#7015,#7016);
#5985=AXIS2_PLACEMENT_3D('',#8803,#7020,#7021);
#5986=AXIS2_PLACEMENT_3D('',#8805,#7022,#7023);
#5987=AXIS2_PLACEMENT_3D('',#8808,#7025,#7026);
#5988=AXIS2_PLACEMENT_3D('',#8809,#7027,#7028);
#5989=AXIS2_PLACEMENT_3D('',#8811,#7029,#7030);
#5990=AXIS2_PLACEMENT_3D('',#8814,#7032,#7033);
#5991=AXIS2_PLACEMENT_3D('',#8815,#7034,#7035);
#5992=AXIS2_PLACEMENT_3D('',#8824,#7040,#7041);
#5993=AXIS2_PLACEMENT_3D('',#8827,#7044,#7045);
#5994=AXIS2_PLACEMENT_3D('',#8830,#7048,#7049);
#5995=AXIS2_PLACEMENT_3D('',#8839,#7054,#7055);
#5996=AXIS2_PLACEMENT_3D('',#8845,#7059,#7060);
#5997=AXIS2_PLACEMENT_3D('',#8848,#7063,#7064);
#5998=AXIS2_PLACEMENT_3D('',#8850,#7065,#7066);
#5999=AXIS2_PLACEMENT_3D('',#8853,#7068,#7069);
#6000=AXIS2_PLACEMENT_3D('',#8854,#7070,#7071);
#6001=AXIS2_PLACEMENT_3D('',#8863,#7076,#7077);
#6002=AXIS2_PLACEMENT_3D('',#8869,#7081,#7082);
#6003=AXIS2_PLACEMENT_3D('',#8875,#7086,#7087);
#6004=AXIS2_PLACEMENT_3D('',#8877,#7088,#7089);
#6005=AXIS2_PLACEMENT_3D('',#8880,#7091,#7092);
#6006=AXIS2_PLACEMENT_3D('',#8881,#7093,#7094);
#6007=AXIS2_PLACEMENT_3D('',#8883,#7095,#7096);
#6008=AXIS2_PLACEMENT_3D('',#8886,#7098,#7099);
#6009=AXIS2_PLACEMENT_3D('',#8887,#7100,#7101);
#6010=AXIS2_PLACEMENT_3D('',#8896,#7106,#7107);
#6011=AXIS2_PLACEMENT_3D('',#8902,#7111,#7112);
#6012=AXIS2_PLACEMENT_3D('',#8908,#7116,#7117);
#6013=AXIS2_PLACEMENT_3D('',#8910,#7118,#7119);
#6014=AXIS2_PLACEMENT_3D('',#8913,#7121,#7122);
#6015=AXIS2_PLACEMENT_3D('',#8914,#7123,#7124);
#6016=AXIS2_PLACEMENT_3D('',#8916,#7125,#7126);
#6017=AXIS2_PLACEMENT_3D('',#8919,#7128,#7129);
#6018=AXIS2_PLACEMENT_3D('',#8920,#7130,#7131);
#6019=AXIS2_PLACEMENT_3D('',#8929,#7136,#7137);
#6020=AXIS2_PLACEMENT_3D('',#8932,#7140,#7141);
#6021=AXIS2_PLACEMENT_3D('',#8935,#7144,#7145);
#6022=AXIS2_PLACEMENT_3D('',#8944,#7150,#7151);
#6023=AXIS2_PLACEMENT_3D('',#8947,#7154,#7155);
#6024=AXIS2_PLACEMENT_3D('',#8950,#7158,#7159);
#6025=AXIS2_PLACEMENT_3D('',#8959,#7164,#7165);
#6026=AXIS2_PLACEMENT_3D('',#8965,#7169,#7170);
#6027=AXIS2_PLACEMENT_3D('',#8968,#7173,#7174);
#6028=AXIS2_PLACEMENT_3D('',#8970,#7175,#7176);
#6029=AXIS2_PLACEMENT_3D('',#8973,#7178,#7179);
#6030=AXIS2_PLACEMENT_3D('',#8974,#7180,#7181);
#6031=AXIS2_PLACEMENT_3D('',#8983,#7186,#7187);
#6032=AXIS2_PLACEMENT_3D('',#8989,#7191,#7192);
#6033=AXIS2_PLACEMENT_3D('',#8992,#7195,#7196);
#6034=AXIS2_PLACEMENT_3D('',#8994,#7197,#7198);
#6035=AXIS2_PLACEMENT_3D('',#8997,#7200,#7201);
#6036=AXIS2_PLACEMENT_3D('',#8998,#7202,#7203);
#6037=AXIS2_PLACEMENT_3D('',#9007,#7208,#7209);
#6038=AXIS2_PLACEMENT_3D('',#9013,#7213,#7214);
#6039=AXIS2_PLACEMENT_3D('',#9019,#7218,#7219);
#6040=AXIS2_PLACEMENT_3D('',#9021,#7220,#7221);
#6041=AXIS2_PLACEMENT_3D('',#9024,#7223,#7224);
#6042=AXIS2_PLACEMENT_3D('',#9025,#7225,#7226);
#6043=AXIS2_PLACEMENT_3D('',#9027,#7227,#7228);
#6044=AXIS2_PLACEMENT_3D('',#9030,#7230,#7231);
#6045=AXIS2_PLACEMENT_3D('',#9031,#7232,#7233);
#6046=AXIS2_PLACEMENT_3D('',#9040,#7238,#7239);
#6047=AXIS2_PLACEMENT_3D('',#9046,#7243,#7244);
#6048=AXIS2_PLACEMENT_3D('',#9049,#7247,#7248);
#6049=AXIS2_PLACEMENT_3D('',#9051,#7249,#7250);
#6050=AXIS2_PLACEMENT_3D('',#9054,#7252,#7253);
#6051=AXIS2_PLACEMENT_3D('',#9055,#7254,#7255);
#6052=AXIS2_PLACEMENT_3D('',#9064,#7260,#7261);
#6053=AXIS2_PLACEMENT_3D('',#9070,#7265,#7266);
#6054=AXIS2_PLACEMENT_3D('',#9073,#7269,#7270);
#6055=AXIS2_PLACEMENT_3D('',#9075,#7271,#7272);
#6056=AXIS2_PLACEMENT_3D('',#9078,#7274,#7275);
#6057=AXIS2_PLACEMENT_3D('',#9079,#7276,#7277);
#6058=AXIS2_PLACEMENT_3D('',#9088,#7282,#7283);
#6059=AXIS2_PLACEMENT_3D('',#9091,#7286,#7287);
#6060=AXIS2_PLACEMENT_3D('',#9094,#7290,#7291);
#6061=AXIS2_PLACEMENT_3D('',#9103,#7296,#7297);
#6062=AXIS2_PLACEMENT_3D('',#9109,#7301,#7302);
#6063=AXIS2_PLACEMENT_3D('',#9115,#7306,#7307);
#6064=AXIS2_PLACEMENT_3D('',#9117,#7308,#7309);
#6065=AXIS2_PLACEMENT_3D('',#9120,#7311,#7312);
#6066=AXIS2_PLACEMENT_3D('',#9121,#7313,#7314);
#6067=AXIS2_PLACEMENT_3D('',#9123,#7315,#7316);
#6068=AXIS2_PLACEMENT_3D('',#9126,#7318,#7319);
#6069=AXIS2_PLACEMENT_3D('',#9127,#7320,#7321);
#6070=AXIS2_PLACEMENT_3D('',#9136,#7326,#7327);
#6071=AXIS2_PLACEMENT_3D('',#9139,#7330,#7331);
#6072=AXIS2_PLACEMENT_3D('',#9142,#7334,#7335);
#6073=AXIS2_PLACEMENT_3D('',#9151,#7340,#7341);
#6074=AXIS2_PLACEMENT_3D('',#9157,#7345,#7346);
#6075=AXIS2_PLACEMENT_3D('',#9163,#7350,#7351);
#6076=AXIS2_PLACEMENT_3D('',#9165,#7352,#7353);
#6077=AXIS2_PLACEMENT_3D('',#9168,#7355,#7356);
#6078=AXIS2_PLACEMENT_3D('',#9169,#7357,#7358);
#6079=AXIS2_PLACEMENT_3D('',#9171,#7359,#7360);
#6080=AXIS2_PLACEMENT_3D('',#9174,#7362,#7363);
#6081=AXIS2_PLACEMENT_3D('',#9175,#7364,#7365);
#6082=AXIS2_PLACEMENT_3D('',#9184,#7370,#7371);
#6083=AXIS2_PLACEMENT_3D('',#9187,#7374,#7375);
#6084=AXIS2_PLACEMENT_3D('',#9190,#7378,#7379);
#6085=AXIS2_PLACEMENT_3D('',#9199,#7384,#7385);
#6086=AXIS2_PLACEMENT_3D('',#9205,#7389,#7390);
#6087=AXIS2_PLACEMENT_3D('',#9211,#7394,#7395);
#6088=AXIS2_PLACEMENT_3D('',#9213,#7396,#7397);
#6089=AXIS2_PLACEMENT_3D('',#9216,#7399,#7400);
#6090=AXIS2_PLACEMENT_3D('',#9217,#7401,#7402);
#6091=AXIS2_PLACEMENT_3D('',#9219,#7403,#7404);
#6092=AXIS2_PLACEMENT_3D('',#9222,#7406,#7407);
#6093=AXIS2_PLACEMENT_3D('',#9223,#7408,#7409);
#6094=AXIS2_PLACEMENT_3D('',#9232,#7414,#7415);
#6095=AXIS2_PLACEMENT_3D('',#9238,#7419,#7420);
#6096=AXIS2_PLACEMENT_3D('',#9241,#7423,#7424);
#6097=AXIS2_PLACEMENT_3D('',#9243,#7425,#7426);
#6098=AXIS2_PLACEMENT_3D('',#9246,#7428,#7429);
#6099=AXIS2_PLACEMENT_3D('',#9247,#7430,#7431);
#6100=AXIS2_PLACEMENT_3D('',#9256,#7436,#7437);
#6101=AXIS2_PLACEMENT_3D('',#9262,#7441,#7442);
#6102=AXIS2_PLACEMENT_3D('',#9265,#7445,#7446);
#6103=AXIS2_PLACEMENT_3D('',#9267,#7447,#7448);
#6104=AXIS2_PLACEMENT_3D('',#9270,#7450,#7451);
#6105=AXIS2_PLACEMENT_3D('',#9271,#7452,#7453);
#6106=AXIS2_PLACEMENT_3D('',#9280,#7458,#7459);
#6107=AXIS2_PLACEMENT_3D('',#9283,#7462,#7463);
#6108=AXIS2_PLACEMENT_3D('',#9289,#7467,#7468);
#6109=AXIS2_PLACEMENT_3D('',#9291,#7469,#7470);
#6110=AXIS2_PLACEMENT_3D('',#9294,#7472,#7473);
#6111=AXIS2_PLACEMENT_3D('',#9295,#7474,#7475);
#6112=AXIS2_PLACEMENT_3D('',#9304,#7480,#7481);
#6113=AXIS2_PLACEMENT_3D('',#9310,#7485,#7486);
#6114=AXIS2_PLACEMENT_3D('',#9316,#7490,#7491);
#6115=AXIS2_PLACEMENT_3D('',#9318,#7492,#7493);
#6116=AXIS2_PLACEMENT_3D('',#9321,#7495,#7496);
#6117=AXIS2_PLACEMENT_3D('',#9322,#7497,#7498);
#6118=AXIS2_PLACEMENT_3D('',#9324,#7499,#7500);
#6119=AXIS2_PLACEMENT_3D('',#9327,#7502,#7503);
#6120=AXIS2_PLACEMENT_3D('',#9328,#7504,#7505);
#6121=AXIS2_PLACEMENT_3D('',#9337,#7510,#7511);
#6122=AXIS2_PLACEMENT_3D('',#9340,#7514,#7515);
#6123=AXIS2_PLACEMENT_3D('',#9343,#7518,#7519);
#6124=AXIS2_PLACEMENT_3D('',#9352,#7524,#7525);
#6125=AXIS2_PLACEMENT_3D('',#9355,#7528,#7529);
#6126=AXIS2_PLACEMENT_3D('',#9358,#7532,#7533);
#6127=AXIS2_PLACEMENT_3D('',#9367,#7538,#7539);
#6128=AXIS2_PLACEMENT_3D('',#9370,#7542,#7543);
#6129=AXIS2_PLACEMENT_3D('',#9373,#7546,#7547);
#6130=AXIS2_PLACEMENT_3D('',#9382,#7552,#7553);
#6131=AXIS2_PLACEMENT_3D('',#9391,#7558,#7559);
#6132=AXIS2_PLACEMENT_3D('',#9393,#7560,#7561);
#6133=AXIS2_PLACEMENT_3D('',#9396,#7563,#7564);
#6134=AXIS2_PLACEMENT_3D('',#9397,#7565,#7566);
#6135=AXIS2_PLACEMENT_3D('',#9399,#7567,#7568);
#6136=AXIS2_PLACEMENT_3D('',#9402,#7570,#7571);
#6137=AXIS2_PLACEMENT_3D('',#9403,#7572,#7573);
#6138=AXIS2_PLACEMENT_3D('',#9405,#7574,#7575);
#6139=AXIS2_PLACEMENT_3D('',#9408,#7577,#7578);
#6140=AXIS2_PLACEMENT_3D('',#9409,#7579,#7580);
#6141=AXIS2_PLACEMENT_3D('',#9411,#7581,#7582);
#6142=AXIS2_PLACEMENT_3D('',#9414,#7584,#7585);
#6143=AXIS2_PLACEMENT_3D('',#9415,#7586,#7587);
#6144=AXIS2_PLACEMENT_3D('',#9418,#7590,#7591);
#6145=AXIS2_PLACEMENT_3D('',#9427,#7596,#7597);
#6146=AXIS2_PLACEMENT_3D('',#9429,#7598,#7599);
#6147=AXIS2_PLACEMENT_3D('',#9432,#7601,#7602);
#6148=AXIS2_PLACEMENT_3D('',#9433,#7603,#7604);
#6149=AXIS2_PLACEMENT_3D('',#9435,#7605,#7606);
#6150=AXIS2_PLACEMENT_3D('',#9438,#7608,#7609);
#6151=AXIS2_PLACEMENT_3D('',#9439,#7610,#7611);
#6152=AXIS2_PLACEMENT_3D('',#9442,#7614,#7615);
#6153=AXIS2_PLACEMENT_3D('',#9451,#7620,#7621);
#6154=AXIS2_PLACEMENT_3D('',#9453,#7622,#7623);
#6155=AXIS2_PLACEMENT_3D('',#9456,#7625,#7626);
#6156=AXIS2_PLACEMENT_3D('',#9457,#7627,#7628);
#6157=AXIS2_PLACEMENT_3D('',#9459,#7629,#7630);
#6158=AXIS2_PLACEMENT_3D('',#9462,#7632,#7633);
#6159=AXIS2_PLACEMENT_3D('',#9463,#7634,#7635);
#6160=AXIS2_PLACEMENT_3D('',#9466,#7638,#7639);
#6161=AXIS2_PLACEMENT_3D('',#9475,#7644,#7645);
#6162=AXIS2_PLACEMENT_3D('',#9477,#7646,#7647);
#6163=AXIS2_PLACEMENT_3D('',#9480,#7649,#7650);
#6164=AXIS2_PLACEMENT_3D('',#9481,#7651,#7652);
#6165=AXIS2_PLACEMENT_3D('',#9483,#7653,#7654);
#6166=AXIS2_PLACEMENT_3D('',#9486,#7656,#7657);
#6167=AXIS2_PLACEMENT_3D('',#9487,#7658,#7659);
#6168=AXIS2_PLACEMENT_3D('',#9490,#7662,#7663);
#6169=AXIS2_PLACEMENT_3D('',#9499,#7668,#7669);
#6170=AXIS2_PLACEMENT_3D('',#9501,#7670,#7671);
#6171=AXIS2_PLACEMENT_3D('',#9504,#7673,#7674);
#6172=AXIS2_PLACEMENT_3D('',#9505,#7675,#7676);
#6173=AXIS2_PLACEMENT_3D('',#9507,#7677,#7678);
#6174=AXIS2_PLACEMENT_3D('',#9510,#7680,#7681);
#6175=AXIS2_PLACEMENT_3D('',#9511,#7682,#7683);
#6176=AXIS2_PLACEMENT_3D('',#9514,#7686,#7687);
#6177=AXIS2_PLACEMENT_3D('',#9517,#7690,#7691);
#6178=AXIS2_PLACEMENT_3D('',#9519,#7692,#7693);
#6179=AXIS2_PLACEMENT_3D('',#9522,#7695,#7696);
#6180=AXIS2_PLACEMENT_3D('',#9523,#7697,#7698);
#6181=AXIS2_PLACEMENT_3D('',#9524,#7699,#7700);
#6182=AXIS2_PLACEMENT_3D('',#9525,#7701,#7702);
#6183=AXIS2_PLACEMENT_3D('',#9526,#7703,#7704);
#6184=AXIS2_PLACEMENT_3D('',#9528,#7705,#7706);
#6185=AXIS2_PLACEMENT_3D('',#9531,#7708,#7709);
#6186=AXIS2_PLACEMENT_3D('',#9532,#7710,#7711);
#6187=AXIS2_PLACEMENT_3D('',#9534,#7712,#7713);
#6188=AXIS2_PLACEMENT_3D('',#9535,#7714,#7715);
#6189=AXIS2_PLACEMENT_3D('',#9544,#7719,#7720);
#6190=AXIS2_PLACEMENT_3D('',#9548,#7722,#7723);
#6191=AXIS2_PLACEMENT_3D('',#9552,#7725,#7726);
#6192=AXIS2_PLACEMENT_3D('',#9556,#7728,#7729);
#6193=AXIS2_PLACEMENT_3D('',#9564,#7733,#7734);
#6194=AXIS2_PLACEMENT_3D('',#9567,#7736,#7737);
#6195=AXIS2_PLACEMENT_3D('',#9568,#7738,#7739);
#6196=AXIS2_PLACEMENT_3D('',#9574,#7743,#7744);
#6197=AXIS2_PLACEMENT_3D('',#9577,#7745,#7746);
#6198=AXIS2_PLACEMENT_3D('',#9580,#7749,#7750);
#6199=AXIS2_PLACEMENT_3D('',#9584,#7753,#7754);
#6200=AXIS2_PLACEMENT_3D('',#9586,#7755,#7756);
#6201=AXIS2_PLACEMENT_3D('',#9588,#7758,#7759);
#6202=AXIS2_PLACEMENT_3D('',#9592,#7762,#7763);
#6203=AXIS2_PLACEMENT_3D('',#9594,#7765,#7766);
#6204=AXIS2_PLACEMENT_3D('',#9600,#7769,#7770);
#6205=AXIS2_PLACEMENT_3D('',#9604,#7772,#7773);
#6206=AXIS2_PLACEMENT_3D('',#9608,#7775,#7776);
#6207=AXIS2_PLACEMENT_3D('',#9612,#7778,#7779);
#6208=AXIS2_PLACEMENT_3D('',#9615,#7781,#7782);
#6209=AXIS2_PLACEMENT_3D('',#9616,#7783,#7784);
#6210=AXIS2_PLACEMENT_3D('',#9618,#7786,#7787);
#6211=AXIS2_PLACEMENT_3D('',#9620,#7789,#7790);
#6212=AXIS2_PLACEMENT_3D('',#9622,#7792,#7793);
#6213=AXIS2_PLACEMENT_3D('',#9624,#7795,#7796);
#6214=AXIS2_PLACEMENT_3D('',#9626,#7798,#7799);
#6215=AXIS2_PLACEMENT_3D('',#9628,#7801,#7802);
#6216=AXIS2_PLACEMENT_3D('',#9630,#7804,#7805);
#6217=AXIS2_PLACEMENT_3D('',#9632,#7807,#7808);
#6218=AXIS2_PLACEMENT_3D('',#9634,#7810,#7811);
#6219=AXIS2_PLACEMENT_3D('',#9636,#7813,#7814);
#6220=AXIS2_PLACEMENT_3D('',#9637,#7815,#7816);
#6221=AXIS2_PLACEMENT_3D('',#9638,#7817,#7818);
#6222=AXIS2_PLACEMENT_3D('',#9640,#7819,#7820);
#6223=AXIS2_PLACEMENT_3D('',#9643,#7822,#7823);
#6224=AXIS2_PLACEMENT_3D('',#9644,#7824,#7825);
#6225=AXIS2_PLACEMENT_3D('',#9646,#7826,#7827);
#6226=AXIS2_PLACEMENT_3D('',#9649,#7829,#7830);
#6227=AXIS2_PLACEMENT_3D('',#9650,#7831,#7832);
#6228=AXIS2_PLACEMENT_3D('',#9653,#7833,#7834);
#6229=AXIS2_PLACEMENT_3D('',#9654,#7835,#7836);
#6230=AXIS2_PLACEMENT_3D('',#9657,#7838,#7839);
#6231=AXIS2_PLACEMENT_3D('',#9658,#7840,#7841);
#6232=AXIS2_PLACEMENT_3D('',#9661,#7843,#7844);
#6233=AXIS2_PLACEMENT_3D('',#9662,#7845,#7846);
#6234=AXIS2_PLACEMENT_3D('',#9664,#7847,#7848);
#6235=AXIS2_PLACEMENT_3D('',#9666,#7849,#7850);
#6236=AXIS2_PLACEMENT_3D('',#9667,#7851,#7852);
#6237=AXIS2_PLACEMENT_3D('',#9668,#7853,#7854);
#6238=AXIS2_PLACEMENT_3D('',#9670,#7855,#7856);
#6239=AXIS2_PLACEMENT_3D('',#9672,#7858,#7859);
#6240=AXIS2_PLACEMENT_3D('',#9674,#7860,#7861);
#6241=AXIS2_PLACEMENT_3D('',#9675,#7862,#7863);
#6242=AXIS2_PLACEMENT_3D('',#9676,#7864,#7865);
#6243=AXIS2_PLACEMENT_3D('',#9679,#7867,#7868);
#6244=AXIS2_PLACEMENT_3D('',#9680,#7869,#7870);
#6245=AXIS2_PLACEMENT_3D('',#9681,#7871,#7872);
#6246=AXIS2_PLACEMENT_3D('',#9682,#7873,#7874);
#6247=AXIS2_PLACEMENT_3D('',#9683,#7875,#7876);
#6248=AXIS2_PLACEMENT_3D('',#9684,#7877,#7878);
#6249=AXIS2_PLACEMENT_3D('',#9687,#7879,#7880);
#6250=AXIS2_PLACEMENT_3D('',#9690,#7882,#7883);
#6251=AXIS2_PLACEMENT_3D('',#9691,#7884,#7885);
#6252=AXIS2_PLACEMENT_3D('',#9692,#7886,#7887);
#6253=AXIS2_PLACEMENT_3D('',#9695,#7889,#7890);
#6254=AXIS2_PLACEMENT_3D('',#9696,#7891,#7892);
#6255=AXIS2_PLACEMENT_3D('',#9698,#7893,#7894);
#6256=AXIS2_PLACEMENT_3D('',#9699,#7895,#7896);
#6257=AXIS2_PLACEMENT_3D('',#9700,#7897,#7898);
#6258=AXIS2_PLACEMENT_3D('',#9702,#7899,#7900);
#6259=AXIS2_PLACEMENT_3D('',#9705,#7902,#7903);
#6260=AXIS2_PLACEMENT_3D('',#9706,#7904,#7905);
#6261=AXIS2_PLACEMENT_3D('',#9708,#7906,#7907);
#6262=AXIS2_PLACEMENT_3D('',#9710,#7908,#7909);
#6263=AXIS2_PLACEMENT_3D('',#9711,#7910,#7911);
#6264=AXIS2_PLACEMENT_3D('',#9712,#7912,#7913);
#6265=AXIS2_PLACEMENT_3D('',#9715,#7915,#7916);
#6266=AXIS2_PLACEMENT_3D('',#9716,#7917,#7918);
#6267=AXIS2_PLACEMENT_3D('',#9719,#7920,#7921);
#6268=AXIS2_PLACEMENT_3D('',#9720,#7922,#7923);
#6269=AXIS2_PLACEMENT_3D('',#9722,#7924,#7925);
#6270=AXIS2_PLACEMENT_3D('',#9724,#7926,#7927);
#6271=AXIS2_PLACEMENT_3D('',#9725,#7928,#7929);
#6272=AXIS2_PLACEMENT_3D('',#9726,#7930,#7931);
#6273=AXIS2_PLACEMENT_3D('',#9729,#7933,#7934);
#6274=AXIS2_PLACEMENT_3D('',#9730,#7935,#7936);
#6275=AXIS2_PLACEMENT_3D('',#9732,#7937,#7938);
#6276=AXIS2_PLACEMENT_3D('',#9733,#7939,#7940);
#6277=AXIS2_PLACEMENT_3D('',#9734,#7941,#7942);
#6278=AXIS2_PLACEMENT_3D('',#9735,#7943,#7944);
#6279=AXIS2_PLACEMENT_3D('',#9736,#7945,#7946);
#6280=AXIS2_PLACEMENT_3D('',#9737,#7947,#7948);
#6281=AXIS2_PLACEMENT_3D('',#9738,#7949,#7950);
#6282=AXIS2_PLACEMENT_3D('',#9740,#7951,#7952);
#6283=AXIS2_PLACEMENT_3D('',#9743,#7954,#7955);
#6284=AXIS2_PLACEMENT_3D('',#9744,#7956,#7957);
#6285=AXIS2_PLACEMENT_3D('',#9746,#7958,#7959);
#6286=AXIS2_PLACEMENT_3D('',#9748,#7960,#7961);
#6287=AXIS2_PLACEMENT_3D('',#9749,#7962,#7963);
#6288=AXIS2_PLACEMENT_3D('',#9750,#7964,#7965);
#6289=AXIS2_PLACEMENT_3D('',#9752,#7966,#7967);
#6290=AXIS2_PLACEMENT_3D('',#9754,#7969,#7970);
#6291=AXIS2_PLACEMENT_3D('',#9756,#7971,#7972);
#6292=AXIS2_PLACEMENT_3D('',#9757,#7973,#7974);
#6293=AXIS2_PLACEMENT_3D('',#9758,#7975,#7976);
#6294=AXIS2_PLACEMENT_3D('',#9760,#7977,#7978);
#6295=AXIS2_PLACEMENT_3D('',#9762,#7979,#7980);
#6296=AXIS2_PLACEMENT_3D('',#9763,#7981,#7982);
#6297=AXIS2_PLACEMENT_3D('',#9764,#7983,#7984);
#6298=AXIS2_PLACEMENT_3D('',#9766,#7985,#7986);
#6299=AXIS2_PLACEMENT_3D('',#9768,#7988,#7989);
#6300=AXIS2_PLACEMENT_3D('',#9770,#7990,#7991);
#6301=AXIS2_PLACEMENT_3D('',#9771,#7992,#7993);
#6302=AXIS2_PLACEMENT_3D('',#9772,#7994,#7995);
#6303=AXIS2_PLACEMENT_3D('',#9774,#7996,#7997);
#6304=AXIS2_PLACEMENT_3D('',#9776,#7998,#7999);
#6305=AXIS2_PLACEMENT_3D('',#9777,#8000,#8001);
#6306=AXIS2_PLACEMENT_3D('',#9778,#8002,#8003);
#6307=AXIS2_PLACEMENT_3D('',#9780,#8004,#8005);
#6308=AXIS2_PLACEMENT_3D('',#9782,#8007,#8008);
#6309=AXIS2_PLACEMENT_3D('',#9784,#8009,#8010);
#6310=AXIS2_PLACEMENT_3D('',#9785,#8011,#8012);
#6311=AXIS2_PLACEMENT_3D('',#9786,#8013,#8014);
#6312=AXIS2_PLACEMENT_3D('',#9788,#8015,#8016);
#6313=AXIS2_PLACEMENT_3D('',#9790,#8017,#8018);
#6314=AXIS2_PLACEMENT_3D('',#9791,#8019,#8020);
#6315=AXIS2_PLACEMENT_3D('',#9792,#8021,#8022);
#6316=AXIS2_PLACEMENT_3D('',#9794,#8023,#8024);
#6317=AXIS2_PLACEMENT_3D('',#9796,#8026,#8027);
#6318=AXIS2_PLACEMENT_3D('',#9797,#8028,#8029);
#6319=AXIS2_PLACEMENT_3D('',#9798,#8030,#8031);
#6320=AXIS2_PLACEMENT_3D('',#9799,#8032,#8033);
#6321=AXIS2_PLACEMENT_3D('',#9800,#8034,#8035);
#6322=AXIS2_PLACEMENT_3D('',#9801,#8036,#8037);
#6323=AXIS2_PLACEMENT_3D('',#9803,#8038,#8039);
#6324=AXIS2_PLACEMENT_3D('',#9806,#8041,#8042);
#6325=AXIS2_PLACEMENT_3D('',#9807,#8043,#8044);
#6326=AXIS2_PLACEMENT_3D('',#9809,#8045,#8046);
#6327=AXIS2_PLACEMENT_3D('',#9811,#8047,#8048);
#6328=AXIS2_PLACEMENT_3D('',#9812,#8049,#8050);
#6329=AXIS2_PLACEMENT_3D('',#9813,#8051,#8052);
#6330=AXIS2_PLACEMENT_3D('',#9815,#8053,#8054);
#6331=AXIS2_PLACEMENT_3D('',#9817,#8056,#8057);
#6332=AXIS2_PLACEMENT_3D('',#9819,#8058,#8059);
#6333=AXIS2_PLACEMENT_3D('',#9820,#8060,#8061);
#6334=AXIS2_PLACEMENT_3D('',#9821,#8062,#8063);
#6335=AXIS2_PLACEMENT_3D('',#9823,#8064,#8065);
#6336=AXIS2_PLACEMENT_3D('',#9825,#8066,#8067);
#6337=AXIS2_PLACEMENT_3D('',#9826,#8068,#8069);
#6338=AXIS2_PLACEMENT_3D('',#9827,#8070,#8071);
#6339=AXIS2_PLACEMENT_3D('',#9829,#8072,#8073);
#6340=AXIS2_PLACEMENT_3D('',#9831,#8075,#8076);
#6341=AXIS2_PLACEMENT_3D('',#9833,#8077,#8078);
#6342=AXIS2_PLACEMENT_3D('',#9834,#8079,#8080);
#6343=AXIS2_PLACEMENT_3D('',#9835,#8081,#8082);
#6344=AXIS2_PLACEMENT_3D('',#9837,#8083,#8084);
#6345=AXIS2_PLACEMENT_3D('',#9839,#8085,#8086);
#6346=AXIS2_PLACEMENT_3D('',#9840,#8087,#8088);
#6347=AXIS2_PLACEMENT_3D('',#9841,#8089,#8090);
#6348=AXIS2_PLACEMENT_3D('',#9843,#8091,#8092);
#6349=AXIS2_PLACEMENT_3D('',#9845,#8094,#8095);
#6350=AXIS2_PLACEMENT_3D('',#9847,#8096,#8097);
#6351=AXIS2_PLACEMENT_3D('',#9848,#8098,#8099);
#6352=AXIS2_PLACEMENT_3D('',#9849,#8100,#8101);
#6353=AXIS2_PLACEMENT_3D('',#9851,#8102,#8103);
#6354=AXIS2_PLACEMENT_3D('',#9853,#8104,#8105);
#6355=AXIS2_PLACEMENT_3D('',#9854,#8106,#8107);
#6356=AXIS2_PLACEMENT_3D('',#9855,#8108,#8109);
#6357=AXIS2_PLACEMENT_3D('',#9857,#8110,#8111);
#6358=AXIS2_PLACEMENT_3D('',#9859,#8113,#8114);
#6359=AXIS2_PLACEMENT_3D('',#9860,#8115,#8116);
#6360=AXIS2_PLACEMENT_3D('',#9861,#8117,#8118);
#6361=AXIS2_PLACEMENT_3D('',#9862,#8119,#8120);
#6362=AXIS2_PLACEMENT_3D('',#9863,#8121,#8122);
#6363=AXIS2_PLACEMENT_3D('',#9864,#8123,#8124);
#6364=AXIS2_PLACEMENT_3D('',#9865,#8125,#8126);
#6365=AXIS2_PLACEMENT_3D('',#9866,#8127,#8128);
#6366=AXIS2_PLACEMENT_3D('',#9867,#8129,#8130);
#6367=AXIS2_PLACEMENT_3D('',#9868,#8131,#8132);
#6368=AXIS2_PLACEMENT_3D('',#9869,#8133,#8134);
#6369=AXIS2_PLACEMENT_3D('',#9870,#8135,#8136);
#6370=AXIS2_PLACEMENT_3D('',#9871,#8137,#8138);
#6371=DIRECTION('axis',(0.,0.,1.));
#6372=DIRECTION('refdir',(1.,0.,0.));
#6373=DIRECTION('axis',(0.,0.,1.));
#6374=DIRECTION('refdir',(1.,0.,0.));
#6375=DIRECTION('center_axis',(-1.,-1.83697019872103E-16,0.));
#6376=DIRECTION('ref_axis',(1.83697019872103E-16,-1.,0.));
#6377=DIRECTION('center_axis',(-1.,-1.83697019872103E-16,0.));
#6378=DIRECTION('ref_axis',(1.83697019872103E-16,-1.,0.));
#6379=DIRECTION('',(-1.,-1.83697019872103E-16,0.));
#6380=DIRECTION('center_axis',(-1.,-1.83697019872103E-16,0.));
#6381=DIRECTION('ref_axis',(1.83697019872103E-16,-1.,0.));
#6382=DIRECTION('center_axis',(-1.,-1.83697019872103E-16,0.));
#6383=DIRECTION('ref_axis',(1.83697019872103E-16,-1.,0.));
#6384=DIRECTION('center_axis',(-1.,-1.83697019872103E-16,0.));
#6385=DIRECTION('ref_axis',(1.83697019872103E-16,-1.,0.));
#6386=DIRECTION('',(-1.,-1.83697019872103E-16,0.));
#6387=DIRECTION('center_axis',(-1.,-1.83697019872103E-16,0.));
#6388=DIRECTION('ref_axis',(1.83697019872103E-16,-1.,0.));
#6389=DIRECTION('center_axis',(-1.,-1.83697019872103E-16,0.));
#6390=DIRECTION('ref_axis',(1.83697019872103E-16,-1.,0.));
#6391=DIRECTION('center_axis',(-1.,-1.83697019872103E-16,0.));
#6392=DIRECTION('ref_axis',(1.83697019872103E-16,-1.,0.));
#6393=DIRECTION('center_axis',(-1.,-1.83697019872103E-16,0.));
#6394=DIRECTION('ref_axis',(1.83697019872103E-16,-1.,0.));
#6395=DIRECTION('',(-1.,-1.83697019872103E-16,0.));
#6396=DIRECTION('center_axis',(-1.,-1.83697019872103E-16,0.));
#6397=DIRECTION('ref_axis',(1.83697019872103E-16,-1.,0.));
#6398=DIRECTION('center_axis',(1.,1.83697019872103E-16,0.));
#6399=DIRECTION('ref_axis',(-1.83697019872103E-16,1.,0.));
#6400=DIRECTION('',(0.707106781186551,-0.707106781186544,-8.6595605623549E-17));
#6401=DIRECTION('center_axis',(-1.,-1.83697019872103E-16,0.));
#6402=DIRECTION('ref_axis',(1.83697019872103E-16,-1.,0.));
#6403=DIRECTION('center_axis',(-1.,-1.83697019872103E-16,0.));
#6404=DIRECTION('ref_axis',(1.85037170770859E-16,-1.,0.));
#6405=DIRECTION('center_axis',(-1.,-1.83697019872103E-16,0.));
#6406=DIRECTION('ref_axis',(1.83697019872103E-16,-1.,0.));
#6407=DIRECTION('center_axis',(2.24963967399279E-32,-1.22464679914735E-16,
-1.));
#6408=DIRECTION('ref_axis',(-1.85037170770859E-16,1.,-1.22464679914735E-16));
#6409=DIRECTION('center_axis',(-1.,-1.83697019872103E-16,0.));
#6410=DIRECTION('ref_axis',(1.83697019872103E-16,-1.,0.));
#6411=DIRECTION('center_axis',(-1.,-1.83697019872103E-16,0.));
#6412=DIRECTION('ref_axis',(1.83697019872103E-16,-1.,0.));
#6413=DIRECTION('center_axis',(-1.,-1.83697019872103E-16,0.));
#6414=DIRECTION('ref_axis',(1.83697019872103E-16,-1.,0.));
#6415=DIRECTION('',(1.,1.83697019872103E-16,0.));
#6416=DIRECTION('center_axis',(-1.,-1.83697019872103E-16,0.));
#6417=DIRECTION('ref_axis',(1.85037170770859E-16,-1.,0.));
#6418=DIRECTION('center_axis',(-1.,-1.83697019872103E-16,0.));
#6419=DIRECTION('ref_axis',(1.83697019872103E-16,-1.,0.));
#6420=DIRECTION('center_axis',(2.24963967399279E-32,-1.22464679914735E-16,
-1.));
#6421=DIRECTION('ref_axis',(-1.85037170770859E-16,1.,-1.22464679914735E-16));
#6422=DIRECTION('center_axis',(-1.,-1.83697019872103E-16,0.));
#6423=DIRECTION('ref_axis',(1.83697019872103E-16,-1.,0.));
#6424=DIRECTION('',(-0.707106781186551,0.707106781186544,-8.6595605623549E-17));
#6425=DIRECTION('center_axis',(-1.,-1.83697019872103E-16,0.));
#6426=DIRECTION('ref_axis',(1.83697019872103E-16,-1.,0.));
#6427=DIRECTION('center_axis',(1.,1.83697019872103E-16,0.));
#6428=DIRECTION('ref_axis',(-1.83697019872103E-16,1.,0.));
#6429=DIRECTION('center_axis',(-1.,-1.83697019872103E-16,0.));
#6430=DIRECTION('ref_axis',(1.83697019872103E-16,-1.,0.));
#6431=DIRECTION('center_axis',(1.,1.83697019872103E-16,0.));
#6432=DIRECTION('ref_axis',(-1.83697019872103E-16,1.,0.));
#6433=DIRECTION('center_axis',(-1.,-1.83697019872103E-16,0.));
#6434=DIRECTION('ref_axis',(1.83697019872103E-16,-1.,0.));
#6435=DIRECTION('center_axis',(1.,1.83697019872103E-16,0.));
#6436=DIRECTION('ref_axis',(-1.83697019872103E-16,1.,0.));
#6437=DIRECTION('center_axis',(-1.,-1.83697019872103E-16,0.));
#6438=DIRECTION('ref_axis',(1.83697019872103E-16,-1.,0.));
#6439=DIRECTION('',(-0.707106781186548,0.707106781186547,8.65956056235493E-17));
#6440=DIRECTION('center_axis',(-1.,-1.83697019872103E-16,0.));
#6441=DIRECTION('ref_axis',(1.83697019872103E-16,-1.,0.));
#6442=DIRECTION('center_axis',(-1.,-1.83697019872103E-16,0.));
#6443=DIRECTION('ref_axis',(1.83697019872103E-16,-1.,0.));
#6444=DIRECTION('center_axis',(-1.,-1.83697019872103E-16,0.));
#6445=DIRECTION('ref_axis',(1.83697019872103E-16,-1.,0.));
#6446=DIRECTION('',(1.,1.83697019872103E-16,0.));
#6447=DIRECTION('center_axis',(-1.,-1.83697019872103E-16,0.));
#6448=DIRECTION('ref_axis',(1.83697019872103E-16,-1.,0.));
#6449=DIRECTION('center_axis',(-1.,-1.83697019872103E-16,0.));
#6450=DIRECTION('ref_axis',(1.96129949112834E-16,-1.,0.));
#6451=DIRECTION('center_axis',(-2.24963967399279E-32,1.22464679914735E-16,
1.));
#6452=DIRECTION('ref_axis',(-1.63441624260695E-16,1.,-1.22464679914735E-16));
#6453=DIRECTION('center_axis',(-1.,-1.83697019872103E-16,0.));
#6454=DIRECTION('ref_axis',(1.83697019872103E-16,-1.,0.));
#6455=DIRECTION('center_axis',(-1.,-1.83697019872103E-16,0.));
#6456=DIRECTION('ref_axis',(1.83697019872103E-16,-1.,0.));
#6457=DIRECTION('center_axis',(-1.,-1.83697019872103E-16,0.));
#6458=DIRECTION('ref_axis',(1.83697019872103E-16,-1.,0.));
#6459=DIRECTION('',(1.,1.83697019872103E-16,0.));
#6460=DIRECTION('center_axis',(-1.,-1.83697019872103E-16,0.));
#6461=DIRECTION('ref_axis',(1.83697019872103E-16,-1.,0.));
#6462=DIRECTION('center_axis',(-1.,-1.83697019872103E-16,0.));
#6463=DIRECTION('ref_axis',(1.96129949112834E-16,-1.,0.));
#6464=DIRECTION('center_axis',(-1.,-1.83697019872103E-16,0.));
#6465=DIRECTION('ref_axis',(1.83697019872103E-16,-1.,0.));
#6466=DIRECTION('center_axis',(-2.24963967399279E-32,1.22464679914735E-16,
1.));
#6467=DIRECTION('ref_axis',(-1.63441624260695E-16,1.,-1.22464679914735E-16));
#6468=DIRECTION('center_axis',(-1.,-1.83697019872103E-16,0.));
#6469=DIRECTION('ref_axis',(1.83697019872103E-16,-1.,0.));
#6470=DIRECTION('center_axis',(-1.,-1.83697019872103E-16,0.));
#6471=DIRECTION('ref_axis',(1.83697019872103E-16,-1.,0.));
#6472=DIRECTION('',(1.,1.83697019872103E-16,0.));
#6473=DIRECTION('center_axis',(-1.,-1.83697019872103E-16,0.));
#6474=DIRECTION('ref_axis',(1.83697019872103E-16,-1.,0.));
#6475=DIRECTION('center_axis',(-1.,-1.83697019872103E-16,0.));
#6476=DIRECTION('ref_axis',(1.83697019872103E-16,-1.,0.));
#6477=DIRECTION('',(0.707106781186548,-0.707106781186547,8.65956056235493E-17));
#6478=DIRECTION('center_axis',(-1.,-1.83697019872103E-16,0.));
#6479=DIRECTION('ref_axis',(1.83697019872103E-16,-1.,0.));
#6480=DIRECTION('center_axis',(-1.,-1.83697019872103E-16,0.));
#6481=DIRECTION('ref_axis',(1.85037170770859E-16,-1.,0.));
#6482=DIRECTION('center_axis',(-1.,-1.83697019872103E-16,0.));
#6483=DIRECTION('ref_axis',(1.83697019872103E-16,-1.,0.));
#6484=DIRECTION('center_axis',(2.24963967399279E-32,-1.22464679914735E-16,
-1.));
#6485=DIRECTION('ref_axis',(-2.31296463463574E-16,1.,-1.22464679914735E-16));
#6486=DIRECTION('center_axis',(-1.,-1.83697019872103E-16,0.));
#6487=DIRECTION('ref_axis',(1.83697019872103E-16,-1.,0.));
#6488=DIRECTION('center_axis',(-1.,-1.83697019872103E-16,0.));
#6489=DIRECTION('ref_axis',(1.83697019872103E-16,-1.,0.));
#6490=DIRECTION('',(-1.,-1.83697019872103E-16,0.));
#6491=DIRECTION('center_axis',(-1.,-1.83697019872103E-16,0.));
#6492=DIRECTION('ref_axis',(1.83697019872103E-16,-1.,0.));
#6493=DIRECTION('center_axis',(-1.,-1.83697019872103E-16,0.));
#6494=DIRECTION('ref_axis',(1.85037170770859E-16,-1.,0.));
#6495=DIRECTION('center_axis',(2.24963967399279E-32,-1.22464679914735E-16,
-1.));
#6496=DIRECTION('ref_axis',(-2.31296463463574E-16,1.,-1.22464679914735E-16));
#6497=DIRECTION('center_axis',(-1.,-1.83697019872103E-16,0.));
#6498=DIRECTION('ref_axis',(1.83697019872103E-16,-1.,0.));
#6499=DIRECTION('center_axis',(-1.,-1.83697019872103E-16,0.));
#6500=DIRECTION('ref_axis',(1.83697019872103E-16,-1.,0.));
#6501=DIRECTION('center_axis',(-1.,-1.83697019872103E-16,0.));
#6502=DIRECTION('ref_axis',(1.83697019872103E-16,-1.,0.));
#6503=DIRECTION('center_axis',(1.,1.83697019872103E-16,0.));
#6504=DIRECTION('ref_axis',(-1.83697019872103E-16,1.,0.));
#6505=DIRECTION('center_axis',(1.,1.83697019872103E-16,0.));
#6506=DIRECTION('ref_axis',(-1.83697019872103E-16,1.,0.));
#6507=DIRECTION('center_axis',(-1.,-1.83697019872103E-16,0.));
#6508=DIRECTION('ref_axis',(1.83697019872103E-16,-1.,0.));
#6509=DIRECTION('center_axis',(-1.,-1.83697019872103E-16,0.));
#6510=DIRECTION('ref_axis',(1.83697019872103E-16,-1.,0.));
#6511=DIRECTION('',(-1.,-1.83697019872103E-16,0.));
#6512=DIRECTION('center_axis',(-1.,-1.83697019872103E-16,0.));
#6513=DIRECTION('ref_axis',(1.83697019872103E-16,-1.,0.));
#6514=DIRECTION('center_axis',(-1.,-1.83697019872103E-16,0.));
#6515=DIRECTION('ref_axis',(1.57361694361665E-16,-1.,0.));
#6516=DIRECTION('center_axis',(-1.,-1.83697019872103E-16,0.));
#6517=DIRECTION('ref_axis',(1.83697019872103E-16,-1.,0.));
#6518=DIRECTION('center_axis',(2.24963967399279E-32,-1.22464679914735E-16,
-1.));
#6519=DIRECTION('ref_axis',(-1.96702117952081E-16,1.,-1.22464679914735E-16));
#6520=DIRECTION('center_axis',(-1.,-1.83697019872103E-16,0.));
#6521=DIRECTION('ref_axis',(1.83697019872103E-16,-1.,0.));
#6522=DIRECTION('center_axis',(-1.,-1.83697019872103E-16,0.));
#6523=DIRECTION('ref_axis',(1.83697019872103E-16,-1.,0.));
#6524=DIRECTION('center_axis',(-1.,-1.83697019872103E-16,0.));
#6525=DIRECTION('ref_axis',(1.83697019872103E-16,-1.,0.));
#6526=DIRECTION('',(0.866025403784443,-0.499999999999992,6.12323399573667E-17));
#6527=DIRECTION('center_axis',(-1.,-1.83697019872103E-16,0.));
#6528=DIRECTION('ref_axis',(2.01689087919369E-16,-1.,0.));
#6529=DIRECTION('center_axis',(-1.,-1.83697019872103E-16,0.));
#6530=DIRECTION('ref_axis',(1.83697019872103E-16,-1.,0.));
#6531=DIRECTION('center_axis',(-2.24963967399279E-32,1.22464679914735E-16,
1.));
#6532=DIRECTION('ref_axis',(-1.89083519924408E-16,1.,-1.22464679914735E-16));
#6533=DIRECTION('center_axis',(-1.,-1.83697019872103E-16,0.));
#6534=DIRECTION('ref_axis',(1.88974131851091E-16,-1.,0.));
#6535=DIRECTION('center_axis',(-1.,-1.83697019872103E-16,0.));
#6536=DIRECTION('ref_axis',(1.83697019872103E-16,-1.,0.));
#6537=DIRECTION('center_axis',(-2.24963967399279E-32,1.22464679914735E-16,
1.));
#6538=DIRECTION('ref_axis',(-1.77163248610397E-16,1.,-1.22464679914735E-16));
#6539=DIRECTION('center_axis',(-1.,-1.83697019872103E-16,0.));
#6540=DIRECTION('ref_axis',(1.83697019872103E-16,-1.,0.));
#6541=DIRECTION('center_axis',(-1.,-1.83697019872103E-16,0.));
#6542=DIRECTION('ref_axis',(1.83697019872103E-16,-1.,0.));
#6543=DIRECTION('center_axis',(-1.,-1.83697019872103E-16,0.));
#6544=DIRECTION('ref_axis',(1.83697019872103E-16,-1.,0.));
#6545=DIRECTION('',(-0.500000000000007,0.866025403784435,-1.0605752387249E-16));
#6546=DIRECTION('center_axis',(-1.,-1.83697019872103E-16,0.));
#6547=DIRECTION('ref_axis',(1.91801449774277E-16,-1.,0.));
#6548=DIRECTION('center_axis',(-1.,-1.83697019872103E-16,0.));
#6549=DIRECTION('ref_axis',(1.83697019872103E-16,-1.,0.));
#6550=DIRECTION('center_axis',(-2.24963967399279E-32,1.22464679914735E-16,
1.));
#6551=DIRECTION('ref_axis',(-1.79813859163385E-16,1.,-1.22464679914735E-16));
#6552=DIRECTION('center_axis',(-1.,-1.83697019872103E-16,0.));
#6553=DIRECTION('ref_axis',(1.87747066251861E-16,-1.,0.));
#6554=DIRECTION('center_axis',(-1.,-1.83697019872103E-16,0.));
#6555=DIRECTION('ref_axis',(1.83697019872103E-16,-1.,0.));
#6556=DIRECTION('center_axis',(2.24963967399279E-32,-1.22464679914735E-16,
-1.));
#6557=DIRECTION('ref_axis',(-1.7601287461112E-16,1.,-1.22464679914735E-16));
#6558=DIRECTION('center_axis',(-1.,-1.83697019872103E-16,0.));
#6559=DIRECTION('ref_axis',(1.83697019872103E-16,-1.,0.));
#6560=DIRECTION('center_axis',(-1.,-1.83697019872103E-16,0.));
#6561=DIRECTION('ref_axis',(1.83697019872103E-16,-1.,0.));
#6562=DIRECTION('center_axis',(-1.,-1.83697019872103E-16,0.));
#6563=DIRECTION('ref_axis',(1.83697019872103E-16,-1.,0.));
#6564=DIRECTION('',(0.500000000000007,-0.866025403784435,1.0605752387249E-16));
#6565=DIRECTION('center_axis',(-1.,-1.83697019872103E-16,0.));
#6566=DIRECTION('ref_axis',(1.85037170770859E-16,-1.,0.));
#6567=DIRECTION('center_axis',(-1.,-1.83697019872103E-16,0.));
#6568=DIRECTION('ref_axis',(1.83697019872103E-16,-1.,0.));
#6569=DIRECTION('center_axis',(2.24963967399279E-32,-1.22464679914735E-16,
-1.));
#6570=DIRECTION('ref_axis',(-1.73472347597681E-16,1.,-1.22464679914735E-16));
#6571=DIRECTION('center_axis',(-1.,-1.83697019872103E-16,0.));
#6572=DIRECTION('ref_axis',(1.97210791246963E-16,-1.,0.));
#6573=DIRECTION('center_axis',(-1.,-1.83697019872103E-16,0.));
#6574=DIRECTION('ref_axis',(1.83697019872103E-16,-1.,0.));
#6575=DIRECTION('center_axis',(2.24963967399279E-32,-1.22464679914735E-16,
-1.));
#6576=DIRECTION('ref_axis',(-1.84885116794028E-16,1.,-1.22464679914735E-16));
#6577=DIRECTION('center_axis',(-1.,-1.83697019872103E-16,0.));
#6578=DIRECTION('ref_axis',(1.83697019872103E-16,-1.,0.));
#6579=DIRECTION('center_axis',(-1.,-1.83697019872103E-16,0.));
#6580=DIRECTION('ref_axis',(1.83697019872103E-16,-1.,0.));
#6581=DIRECTION('center_axis',(-1.,-1.83697019872103E-16,0.));
#6582=DIRECTION('ref_axis',(1.83697019872103E-16,-1.,0.));
#6583=DIRECTION('',(-0.866025403784443,0.499999999999992,-6.12323399573667E-17));
#6584=DIRECTION('center_axis',(1.,1.83697019872103E-16,0.));
#6585=DIRECTION('ref_axis',(-1.83697019872103E-16,1.,0.));
#6586=DIRECTION('center_axis',(1.,1.83697019872103E-16,0.));
#6587=DIRECTION('ref_axis',(-1.83697019872103E-16,1.,0.));
#6588=DIRECTION('center_axis',(-1.,-1.83697019872103E-16,0.));
#6589=DIRECTION('ref_axis',(1.83697019872103E-16,-1.,0.));
#6590=DIRECTION('center_axis',(1.,1.83697019872103E-16,0.));
#6591=DIRECTION('ref_axis',(-1.83697019872103E-16,1.,0.));
#6592=DIRECTION('center_axis',(1.,1.83697019872103E-16,0.));
#6593=DIRECTION('ref_axis',(-1.83697019872103E-16,1.,0.));
#6594=DIRECTION('center_axis',(1.,-1.83697019872103E-16,0.));
#6595=DIRECTION('ref_axis',(-1.83697019872103E-16,-1.,0.));
#6596=DIRECTION('center_axis',(-1.,1.83697019872103E-16,0.));
#6597=DIRECTION('ref_axis',(-1.83697019872103E-16,-1.,0.));
#6598=DIRECTION('',(1.,-1.83697019872103E-16,0.));
#6599=DIRECTION('center_axis',(-1.,1.83697019872103E-16,0.));
#6600=DIRECTION('ref_axis',(-1.83697019872103E-16,-1.,0.));
#6601=DIRECTION('center_axis',(1.,-1.83697019872103E-16,0.));
#6602=DIRECTION('ref_axis',(-1.57361694361665E-16,-1.,0.));
#6603=DIRECTION('center_axis',(-1.,1.83697019872103E-16,0.));
#6604=DIRECTION('ref_axis',(-1.83697019872103E-16,-1.,0.));
#6605=DIRECTION('center_axis',(-2.24963967399279E-32,-1.22464679914735E-16,
1.));
#6606=DIRECTION('ref_axis',(1.96702117952081E-16,1.,1.22464679914735E-16));
#6607=DIRECTION('center_axis',(-1.,1.83697019872103E-16,0.));
#6608=DIRECTION('ref_axis',(-1.83697019872103E-16,-1.,0.));
#6609=DIRECTION('center_axis',(1.,-1.83697019872103E-16,0.));
#6610=DIRECTION('ref_axis',(-1.83697019872103E-16,-1.,0.));
#6611=DIRECTION('center_axis',(-1.,1.83697019872103E-16,0.));
#6612=DIRECTION('ref_axis',(-1.83697019872103E-16,-1.,0.));
#6613=DIRECTION('',(-0.866025403784443,-0.499999999999992,-6.12323399573667E-17));
#6614=DIRECTION('center_axis',(1.,-1.83697019872103E-16,0.));
#6615=DIRECTION('ref_axis',(-2.01689087919369E-16,-1.,0.));
#6616=DIRECTION('center_axis',(-1.,1.83697019872103E-16,0.));
#6617=DIRECTION('ref_axis',(-1.83697019872103E-16,-1.,0.));
#6618=DIRECTION('center_axis',(2.24963967399279E-32,1.22464679914735E-16,
-1.));
#6619=DIRECTION('ref_axis',(1.89083519924408E-16,1.,1.22464679914735E-16));
#6620=DIRECTION('center_axis',(1.,-1.83697019872103E-16,0.));
#6621=DIRECTION('ref_axis',(-1.88974131851091E-16,-1.,0.));
#6622=DIRECTION('center_axis',(-1.,1.83697019872103E-16,0.));
#6623=DIRECTION('ref_axis',(-1.83697019872103E-16,-1.,0.));
#6624=DIRECTION('center_axis',(2.24963967399279E-32,1.22464679914735E-16,
-1.));
#6625=DIRECTION('ref_axis',(1.77163248610397E-16,1.,1.22464679914735E-16));
#6626=DIRECTION('center_axis',(-1.,1.83697019872103E-16,0.));
#6627=DIRECTION('ref_axis',(-1.83697019872103E-16,-1.,0.));
#6628=DIRECTION('center_axis',(1.,-1.83697019872103E-16,0.));
#6629=DIRECTION('ref_axis',(-1.83697019872103E-16,-1.,0.));
#6630=DIRECTION('center_axis',(-1.,1.83697019872103E-16,0.));
#6631=DIRECTION('ref_axis',(-1.83697019872103E-16,-1.,0.));
#6632=DIRECTION('',(0.500000000000007,0.866025403784435,1.0605752387249E-16));
#6633=DIRECTION('center_axis',(1.,-1.83697019872103E-16,0.));
#6634=DIRECTION('ref_axis',(-1.91801449774277E-16,-1.,0.));
#6635=DIRECTION('center_axis',(-1.,1.83697019872103E-16,0.));
#6636=DIRECTION('ref_axis',(-1.83697019872103E-16,-1.,0.));
#6637=DIRECTION('center_axis',(2.24963967399279E-32,1.22464679914735E-16,
-1.));
#6638=DIRECTION('ref_axis',(1.79813859163385E-16,1.,1.22464679914735E-16));
#6639=DIRECTION('center_axis',(1.,-1.83697019872103E-16,0.));
#6640=DIRECTION('ref_axis',(-1.87747066251861E-16,-1.,0.));
#6641=DIRECTION('center_axis',(-1.,1.83697019872103E-16,0.));
#6642=DIRECTION('ref_axis',(-1.83697019872103E-16,-1.,0.));
#6643=DIRECTION('center_axis',(-2.24963967399279E-32,-1.22464679914735E-16,
1.));
#6644=DIRECTION('ref_axis',(1.7601287461112E-16,1.,1.22464679914735E-16));
#6645=DIRECTION('center_axis',(-1.,1.83697019872103E-16,0.));
#6646=DIRECTION('ref_axis',(-1.83697019872103E-16,-1.,0.));
#6647=DIRECTION('center_axis',(1.,-1.83697019872103E-16,0.));
#6648=DIRECTION('ref_axis',(-1.83697019872103E-16,-1.,0.));
#6649=DIRECTION('center_axis',(-1.,1.83697019872103E-16,0.));
#6650=DIRECTION('ref_axis',(-1.83697019872103E-16,-1.,0.));
#6651=DIRECTION('',(-0.500000000000007,-0.866025403784435,-1.0605752387249E-16));
#6652=DIRECTION('center_axis',(1.,-1.83697019872103E-16,0.));
#6653=DIRECTION('ref_axis',(-1.85037170770859E-16,-1.,0.));
#6654=DIRECTION('center_axis',(-1.,1.83697019872103E-16,0.));
#6655=DIRECTION('ref_axis',(-1.83697019872103E-16,-1.,0.));
#6656=DIRECTION('center_axis',(-2.24963967399279E-32,-1.22464679914735E-16,
1.));
#6657=DIRECTION('ref_axis',(1.73472347597681E-16,1.,1.22464679914735E-16));
#6658=DIRECTION('center_axis',(1.,-1.83697019872103E-16,0.));
#6659=DIRECTION('ref_axis',(-1.97210791246963E-16,-1.,0.));
#6660=DIRECTION('center_axis',(-1.,1.83697019872103E-16,0.));
#6661=DIRECTION('ref_axis',(-1.83697019872103E-16,-1.,0.));
#6662=DIRECTION('center_axis',(-2.24963967399279E-32,-1.22464679914735E-16,
1.));
#6663=DIRECTION('ref_axis',(1.84885116794028E-16,1.,1.22464679914735E-16));
#6664=DIRECTION('center_axis',(-1.,1.83697019872103E-16,0.));
#6665=DIRECTION('ref_axis',(-1.83697019872103E-16,-1.,0.));
#6666=DIRECTION('center_axis',(1.,-1.83697019872103E-16,0.));
#6667=DIRECTION('ref_axis',(-1.83697019872103E-16,-1.,0.));
#6668=DIRECTION('center_axis',(-1.,1.83697019872103E-16,0.));
#6669=DIRECTION('ref_axis',(-1.83697019872103E-16,-1.,0.));
#6670=DIRECTION('',(0.866025403784443,0.499999999999992,6.12323399573667E-17));
#6671=DIRECTION('center_axis',(-1.,1.83697019872103E-16,0.));
#6672=DIRECTION('ref_axis',(1.83697019872103E-16,1.,0.));
#6673=DIRECTION('center_axis',(-1.,1.83697019872103E-16,0.));
#6674=DIRECTION('ref_axis',(1.83697019872103E-16,1.,0.));
#6675=DIRECTION('center_axis',(1.,-1.83697019872103E-16,0.));
#6676=DIRECTION('ref_axis',(-1.83697019872103E-16,-1.,0.));
#6677=DIRECTION('center_axis',(-1.,1.83697019872103E-16,0.));
#6678=DIRECTION('ref_axis',(1.83697019872103E-16,1.,0.));
#6679=DIRECTION('center_axis',(-1.,1.83697019872103E-16,0.));
#6680=DIRECTION('ref_axis',(1.83697019872103E-16,1.,0.));
#6681=DIRECTION('axis',(0.,0.,1.));
#6682=DIRECTION('refdir',(1.,0.,0.));
#6683=DIRECTION('center_axis',(0.,0.,1.));
#6684=DIRECTION('ref_axis',(-1.,0.,0.));
#6685=DIRECTION('center_axis',(-1.22514845490924E-16,0.,1.));
#6686=DIRECTION('ref_axis',(-1.,0.,-1.22514845490924E-16));
#6687=DIRECTION('',(-0.737844385259416,-9.0359876467679E-17,-0.67497086095709));
#6688=DIRECTION('center_axis',(1.22514845490924E-16,0.,-1.));
#6689=DIRECTION('ref_axis',(-1.,0.,-1.22514845490924E-16));
#6690=DIRECTION('center_axis',(-8.67361737988404E-17,1.,0.));
#6691=DIRECTION('ref_axis',(1.,8.67361737988404E-17,0.));
#6692=DIRECTION('',(1.,8.67361737988404E-17,0.));
#6693=DIRECTION('',(1.,8.67361737988404E-17,1.22514845490924E-16));
#6694=DIRECTION('center_axis',(1.64798730217797E-16,-1.,0.));
#6695=DIRECTION('ref_axis',(-1.,-1.64798730217797E-16,0.));
#6696=DIRECTION('',(-1.,-1.64798730217797E-16,-1.22514845490924E-16));
#6697=DIRECTION('',(-1.,-1.64798730217797E-16,0.));
#6698=DIRECTION('center_axis',(0.,0.,1.));
#6699=DIRECTION('ref_axis',(1.,0.,0.));
#6700=DIRECTION('center_axis',(6.12574227454618E-17,0.,-1.));
#6701=DIRECTION('ref_axis',(-1.,0.,-6.12574227454618E-17));
#6702=DIRECTION('center_axis',(6.12574227454618E-17,0.,-1.));
#6703=DIRECTION('ref_axis',(-1.,0.,-6.12574227454618E-17));
#6704=DIRECTION('center_axis',(6.12574227454618E-17,0.,-1.));
#6705=DIRECTION('ref_axis',(-1.,0.,-6.12574227454618E-17));
#6706=DIRECTION('center_axis',(-1.22514845490924E-16,0.,1.));
#6707=DIRECTION('ref_axis',(1.,0.,1.22514845490924E-16));
#6708=DIRECTION('center_axis',(1.22514845490924E-16,0.,-1.));
#6709=DIRECTION('ref_axis',(1.,0.,1.22514845490924E-16));
#6710=DIRECTION('center_axis',(-1.22514845490924E-16,0.,1.));
#6711=DIRECTION('ref_axis',(1.,0.,1.22514845490924E-16));
#6712=DIRECTION('center_axis',(1.22514845490924E-16,0.,-1.));
#6713=DIRECTION('ref_axis',(1.,0.,1.22514845490924E-16));
#6714=DIRECTION('center_axis',(1.22514845490924E-16,0.,-1.));
#6715=DIRECTION('ref_axis',(-1.,0.,-1.41469428416086E-16));
#6716=DIRECTION('center_axis',(-1.41689279422427E-16,1.28384806450313E-32,
1.));
#6717=DIRECTION('ref_axis',(1.,-6.12323399573677E-17,1.41689279422427E-16));
#6718=DIRECTION('center_axis',(-1.22464679914735E-16,-1.,-1.50037413378493E-32));
#6719=DIRECTION('ref_axis',(1.,-1.22464679914735E-16,1.06102071312065E-16));
#6720=DIRECTION('center_axis',(1.22514845490924E-16,0.,-1.));
#6721=DIRECTION('ref_axis',(-1.,0.,-1.22514845490924E-16));
#6722=DIRECTION('center_axis',(1.22514845490924E-16,0.,-1.));
#6723=DIRECTION('ref_axis',(1.,0.,1.22514845490924E-16));
#6724=DIRECTION('',(-0.0871557427476016,1.0673500138316E-17,0.99619469809175));
#6725=DIRECTION('center_axis',(1.22514845490924E-16,0.,-1.));
#6726=DIRECTION('ref_axis',(-1.,0.,-1.22514845490924E-16));
#6727=DIRECTION('center_axis',(1.22514845490924E-16,0.,-1.));
#6728=DIRECTION('ref_axis',(-1.,0.,-1.22514845490924E-16));
#6729=DIRECTION('center_axis',(1.22514845490924E-16,0.,-1.));
#6730=DIRECTION('ref_axis',(1.,0.,1.22514845490924E-16));
#6731=DIRECTION('center_axis',(1.22514845490924E-16,0.,-1.));
#6732=DIRECTION('ref_axis',(-1.,0.,-1.22514845490924E-16));
#6733=DIRECTION('center_axis',(1.22514845490924E-16,0.,-1.));
#6734=DIRECTION('ref_axis',(1.,0.,1.22514845490924E-16));
#6735=DIRECTION('',(-1.22514845490924E-16,0.,1.));
#6736=DIRECTION('center_axis',(1.22514845490924E-16,0.,-1.));
#6737=DIRECTION('ref_axis',(-1.,0.,-1.22514845490924E-16));
#6738=DIRECTION('center_axis',(1.22514845490924E-16,0.,-1.));
#6739=DIRECTION('ref_axis',(-1.,0.,-1.22514845490924E-16));
#6740=DIRECTION('',(-0.499999999998812,6.12323399572222E-17,0.866025403785125));
#6741=DIRECTION('center_axis',(1.22514845490924E-16,0.,-1.));
#6742=DIRECTION('ref_axis',(-1.,0.,-1.22514845490924E-16));
#6743=DIRECTION('',(-1.22514845490924E-16,0.,1.));
#6744=DIRECTION('axis',(0.,0.,1.));
#6745=DIRECTION('refdir',(1.,0.,0.));
#6746=DIRECTION('center_axis',(0.,1.,0.));
#6747=DIRECTION('ref_axis',(1.,0.,0.));
#6748=DIRECTION('center_axis',(0.,1.,0.));
#6749=DIRECTION('ref_axis',(1.,0.,0.));
#6750=DIRECTION('',(0.,1.,0.));
#6751=DIRECTION('center_axis',(0.,-1.,0.));
#6752=DIRECTION('ref_axis',(1.,0.,0.));
#6753=DIRECTION('center_axis',(0.,1.,0.));
#6754=DIRECTION('ref_axis',(1.,0.,0.));
#6755=DIRECTION('center_axis',(0.,1.,0.));
#6756=DIRECTION('ref_axis',(1.,0.,0.));
#6757=DIRECTION('',(0.,1.,0.));
#6758=DIRECTION('center_axis',(0.,-1.,0.));
#6759=DIRECTION('ref_axis',(1.,0.,0.));
#6760=DIRECTION('center_axis',(0.,-1.,0.));
#6761=DIRECTION('ref_axis',(1.,0.,0.));
#6762=DIRECTION('center_axis',(0.,-1.,0.));
#6763=DIRECTION('ref_axis',(1.,0.,0.));
#6764=DIRECTION('',(0.,-1.,0.));
#6765=DIRECTION('center_axis',(0.,1.,0.));
#6766=DIRECTION('ref_axis',(1.,0.,0.));
#6767=DIRECTION('center_axis',(0.,-1.,0.));
#6768=DIRECTION('ref_axis',(1.,0.,0.));
#6769=DIRECTION('center_axis',(0.,-1.,0.));
#6770=DIRECTION('ref_axis',(1.,0.,0.));
#6771=DIRECTION('',(0.,1.,0.));
#6772=DIRECTION('center_axis',(0.,1.,0.));
#6773=DIRECTION('ref_axis',(1.,0.,0.));
#6774=DIRECTION('center_axis',(0.,-1.,0.));
#6775=DIRECTION('ref_axis',(1.,0.,0.));
#6776=DIRECTION('center_axis',(0.,1.,0.));
#6777=DIRECTION('ref_axis',(1.,0.,0.));
#6778=DIRECTION('',(0.,0.,-1.));
#6779=DIRECTION('',(1.,0.,0.));
#6780=DIRECTION('',(0.,0.,1.));
#6781=DIRECTION('',(-1.,0.,0.));
#6782=DIRECTION('center_axis',(0.,1.,0.));
#6783=DIRECTION('ref_axis',(1.,0.,0.));
#6784=DIRECTION('center_axis',(0.,-1.,0.));
#6785=DIRECTION('ref_axis',(1.,0.,0.));
#6786=DIRECTION('center_axis',(0.,-1.,0.));
#6787=DIRECTION('ref_axis',(1.,0.,0.));
#6788=DIRECTION('',(0.,-1.,0.));
#6789=DIRECTION('center_axis',(0.,1.,0.));
#6790=DIRECTION('ref_axis',(1.,0.,0.));
#6791=DIRECTION('center_axis',(0.,-1.,0.));
#6792=DIRECTION('ref_axis',(1.,0.,0.));
#6793=DIRECTION('center_axis',(0.,-1.,0.));
#6794=DIRECTION('ref_axis',(1.,0.,0.));
#6795=DIRECTION('',(0.,1.,0.));
#6796=DIRECTION('center_axis',(0.,-1.,0.));
#6797=DIRECTION('ref_axis',(1.,0.,0.));
#6798=DIRECTION('center_axis',(0.,1.,0.));
#6799=DIRECTION('ref_axis',(1.,0.,0.));
#6800=DIRECTION('center_axis',(0.,0.,1.));
#6801=DIRECTION('ref_axis',(1.,0.,0.));
#6802=DIRECTION('',(0.,1.,0.));
#6803=DIRECTION('',(1.,0.,0.));
#6804=DIRECTION('',(0.,1.,0.));
#6805=DIRECTION('center_axis',(-1.,0.,0.));
#6806=DIRECTION('ref_axis',(0.,0.,1.));
#6807=DIRECTION('',(0.,0.,1.));
#6808=DIRECTION('',(0.,1.,0.));
#6809=DIRECTION('center_axis',(0.,0.,-1.));
#6810=DIRECTION('ref_axis',(-1.,0.,0.));
#6811=DIRECTION('',(-1.,0.,0.));
#6812=DIRECTION('',(0.,1.,0.));
#6813=DIRECTION('center_axis',(1.,0.,0.));
#6814=DIRECTION('ref_axis',(0.,0.,-1.));
#6815=DIRECTION('',(0.,0.,-1.));
#6816=DIRECTION('center_axis',(0.,1.,0.));
#6817=DIRECTION('ref_axis',(0.,0.,1.));
#6818=DIRECTION('center_axis',(0.,1.,0.));
#6819=DIRECTION('ref_axis',(1.,0.,0.));
#6820=DIRECTION('axis',(0.,0.,1.));
#6821=DIRECTION('refdir',(1.,0.,0.));
#6822=DIRECTION('center_axis',(-1.38777878078145E-16,-1.,0.));
#6823=DIRECTION('ref_axis',(1.,-1.38777878078145E-16,-1.5395124730131E-48));
#6824=DIRECTION('center_axis',(8.32667268468864E-17,1.,2.13821176807379E-50));
#6825=DIRECTION('ref_axis',(1.,-8.32667268468864E-17,-1.5395124730131E-48));
#6826=DIRECTION('',(-1.38777878078145E-16,-1.,0.));
#6827=DIRECTION('center_axis',(8.32667268468864E-17,1.,2.13821176807379E-50));
#6828=DIRECTION('ref_axis',(1.,-8.32667268468864E-17,-1.5395124730131E-48));
#6829=DIRECTION('center_axis',(-1.38777878078145E-16,-1.,0.));
#6830=DIRECTION('ref_axis',(1.,-1.38777878078145E-16,-1.5395124730131E-48));
#6831=DIRECTION('center_axis',(-8.32667268468864E-17,-1.,-2.13821176807379E-50));
#6832=DIRECTION('ref_axis',(1.,-8.32667268468864E-17,-1.5395124730131E-48));
#6833=DIRECTION('',(1.38777878078145E-16,1.,0.));
#6834=DIRECTION('center_axis',(-8.32667268468864E-17,-1.,-2.13821176807379E-50));
#6835=DIRECTION('ref_axis',(1.,-8.32667268468864E-17,-1.5395124730131E-48));
#6836=DIRECTION('center_axis',(-8.32667268468864E-17,-1.,-2.13821176807379E-50));
#6837=DIRECTION('ref_axis',(1.,-8.32667268468864E-17,-1.5395124730131E-48));
#6838=DIRECTION('center_axis',(-8.32667268468864E-17,-1.,-2.13821176807379E-50));
#6839=DIRECTION('ref_axis',(1.,-8.32667268468864E-17,-1.5395124730131E-48));
#6840=DIRECTION('axis',(0.,0.,1.));
#6841=DIRECTION('refdir',(1.,0.,0.));
#6842=DIRECTION('center_axis',(1.,0.,0.));
#6843=DIRECTION('ref_axis',(0.,0.,-1.));
#6844=DIRECTION('center_axis',(-1.,0.,0.));
#6845=DIRECTION('ref_axis',(0.,1.,0.));
#6846=DIRECTION('center_axis',(0.,-1.,0.));
#6847=DIRECTION('ref_axis',(0.,0.,1.));
#6848=DIRECTION('center_axis',(1.,0.,0.));
#6849=DIRECTION('ref_axis',(0.,1.,0.));
#6850=DIRECTION('center_axis',(1.,0.,0.));
#6851=DIRECTION('ref_axis',(0.,1.,0.));
#6852=DIRECTION('center_axis',(1.,0.,0.));
#6853=DIRECTION('ref_axis',(0.,1.,0.));
#6854=DIRECTION('',(-1.,0.,0.));
#6855=DIRECTION('center_axis',(1.,0.,0.));
#6856=DIRECTION('ref_axis',(0.,1.,0.));
#6857=DIRECTION('center_axis',(-1.,0.,0.));
#6858=DIRECTION('ref_axis',(0.,0.,1.));
#6859=DIRECTION('center_axis',(1.,0.,0.));
#6860=DIRECTION('ref_axis',(0.,1.,0.));
#6861=DIRECTION('center_axis',(0.,-1.,0.));
#6862=DIRECTION('ref_axis',(0.,0.,-1.));
#6863=DIRECTION('center_axis',(-1.,0.,0.));
#6864=DIRECTION('ref_axis',(0.,1.,0.));
#6865=DIRECTION('center_axis',(-1.,0.,0.));
#6866=DIRECTION('ref_axis',(0.,1.,0.));
#6867=DIRECTION('center_axis',(1.,0.,0.));
#6868=DIRECTION('ref_axis',(0.,1.,0.));
#6869=DIRECTION('',(-1.,0.,0.));
#6870=DIRECTION('center_axis',(1.,0.,0.));
#6871=DIRECTION('ref_axis',(0.,1.,0.));
#6872=DIRECTION('center_axis',(-8.32667268468864E-17,-1.,-2.13821176807379E-50));
#6873=DIRECTION('ref_axis',(1.,-8.32667268468864E-17,-1.5395124730131E-48));
#6874=DIRECTION('center_axis',(8.32667268468864E-17,1.,2.13821176807379E-50));
#6875=DIRECTION('ref_axis',(1.,-8.32667268468864E-17,-1.5395124730131E-48));
#6876=DIRECTION('center_axis',(-6.93889390390723E-17,-1.,0.));
#6877=DIRECTION('ref_axis',(1.,-6.93889390390723E-17,-1.5395124730131E-48));
#6878=DIRECTION('center_axis',(-8.32667268468864E-17,-1.,-2.13821176807379E-50));
#6879=DIRECTION('ref_axis',(1.,-8.32667268468864E-17,-1.5395124730131E-48));
#6880=DIRECTION('',(6.93889390390723E-17,1.,0.));
#6881=DIRECTION('',(6.93889390390723E-17,1.,0.));
#6882=DIRECTION('center_axis',(-8.32667268468864E-17,-1.,-2.13821176807379E-50));
#6883=DIRECTION('ref_axis',(1.,-8.32667268468864E-17,-1.5395124730131E-48));
#6884=DIRECTION('axis',(0.,0.,1.));
#6885=DIRECTION('refdir',(1.,0.,0.));
#6886=DIRECTION('center_axis',(0.800546781801578,0.,0.5992702646946));
#6887=DIRECTION('ref_axis',(-0.5992702646946,0.,0.800546781801578));
#6888=DIRECTION('',(0.5992702646946,0.,-0.800546781801578));
#6889=DIRECTION('',(0.,-1.,0.));
#6890=DIRECTION('',(-0.5992702646946,0.,0.800546781801578));
#6891=DIRECTION('',(0.,-1.,0.));
#6892=DIRECTION('center_axis',(0.669128232191225,0.,-0.743146963180666));
#6893=DIRECTION('ref_axis',(0.743146963180666,0.,0.669128232191225));
#6894=DIRECTION('',(-0.743146963180666,0.,-0.669128232191225));
#6895=DIRECTION('',(0.743146963180666,0.,0.669128232191225));
#6896=DIRECTION('',(0.,-1.,0.));
#6897=DIRECTION('center_axis',(-0.490545396583828,0.,0.871415637850512));
#6898=DIRECTION('ref_axis',(-0.871415637850512,0.,-0.490545396583828));
#6899=DIRECTION('',(-0.871415637850512,0.,-0.490545396583828));
#6900=DIRECTION('',(0.,1.,0.));
#6901=DIRECTION('',(-0.871415637850512,0.,-0.490545396583828));
#6902=DIRECTION('center_axis',(0.,-1.,0.));
#6903=DIRECTION('ref_axis',(1.,0.,0.));
#6904=DIRECTION('center_axis',(0.,-1.,0.));
#6905=DIRECTION('ref_axis',(1.,0.,0.));
#6906=DIRECTION('',(0.,1.,0.));
#6907=DIRECTION('center_axis',(0.,-1.,0.));
#6908=DIRECTION('ref_axis',(1.,0.,0.));
#6909=DIRECTION('center_axis',(0.,-1.,0.));
#6910=DIRECTION('ref_axis',(1.,0.,0.));
#6911=DIRECTION('center_axis',(0.,-1.,0.));
#6912=DIRECTION('ref_axis',(1.,0.,0.));
#6913=DIRECTION('',(0.,-1.,0.));
#6914=DIRECTION('center_axis',(0.,-1.,0.));
#6915=DIRECTION('ref_axis',(1.,0.,0.));
#6916=DIRECTION('center_axis',(0.907648207883844,0.,0.419731736619053));
#6917=DIRECTION('ref_axis',(-0.419731736619053,0.,0.907648207883844));
#6918=DIRECTION('',(0.419731736619053,0.,-0.907648207883844));
#6919=DIRECTION('',(0.,-1.,0.));
#6920=DIRECTION('',(-0.419731736619053,0.,0.907648207883844));
#6921=DIRECTION('',(0.,-1.,0.));
#6922=DIRECTION('center_axis',(0.499997233260123,0.,-0.866027001156559));
#6923=DIRECTION('ref_axis',(0.866027001156559,0.,0.499997233260123));
#6924=DIRECTION('',(-0.866027001156559,0.,-0.499997233260123));
#6925=DIRECTION('',(0.866027001156559,0.,0.499997233260123));
#6926=DIRECTION('',(0.,-1.,0.));
#6927=DIRECTION('center_axis',(-0.298648304048949,0.,0.954363238232009));
#6928=DIRECTION('ref_axis',(-0.954363238232009,0.,-0.298648304048949));
#6929=DIRECTION('',(-0.954363238232009,0.,-0.298648304048948));
#6930=DIRECTION('',(-0.954363238232009,0.,-0.298648304048948));
#6931=DIRECTION('center_axis',(0.,-1.,0.));
#6932=DIRECTION('ref_axis',(1.,0.,0.));
#6933=DIRECTION('center_axis',(0.,-1.,0.));
#6934=DIRECTION('ref_axis',(1.,0.,0.));
#6935=DIRECTION('',(0.,1.,0.));
#6936=DIRECTION('center_axis',(0.,-1.,0.));
#6937=DIRECTION('ref_axis',(1.,0.,0.));
#6938=DIRECTION('center_axis',(0.975081051902262,0.,0.221848917556921));
#6939=DIRECTION('ref_axis',(-0.221848917556921,0.,0.975081051902262));
#6940=DIRECTION('',(0.221848917556921,0.,-0.975081051902262));
#6941=DIRECTION('',(0.,-1.,0.));
#6942=DIRECTION('',(-0.221848917556921,0.,0.975081051902262));
#6943=DIRECTION('',(0.,-1.,0.));
#6944=DIRECTION('center_axis',(0.309013955982637,0.,-0.951057503523294));
#6945=DIRECTION('ref_axis',(0.951057503523294,0.,0.309013955982637));
#6946=DIRECTION('',(-0.951057503523294,0.,-0.309013955982637));
#6947=DIRECTION('',(0.951057503523294,0.,0.309013955982637));
#6948=DIRECTION('',(0.,-1.,0.));
#6949=DIRECTION('center_axis',(-0.0936988475535697,0.,0.995600585559858));
#6950=DIRECTION('ref_axis',(-0.995600585559858,0.,-0.0936988475535697));
#6951=DIRECTION('',(-0.995600585559858,0.,-0.0936988475535697));
#6952=DIRECTION('',(-0.995600585559858,0.,-0.0936988475535697));
#6953=DIRECTION('center_axis',(0.,-1.,0.));
#6954=DIRECTION('ref_axis',(1.,0.,0.));
#6955=DIRECTION('center_axis',(0.,-1.,0.));
#6956=DIRECTION('ref_axis',(1.,0.,0.));
#6957=DIRECTION('',(0.,1.,0.));
#6958=DIRECTION('center_axis',(0.,-1.,0.));
#6959=DIRECTION('ref_axis',(1.,0.,0.));
#6960=DIRECTION('center_axis',(0.999898174994542,0.,0.0142702362483363));
#6961=DIRECTION('ref_axis',(-0.0142702362483363,0.,0.999898174994542));
#6962=DIRECTION('',(0.0142702362483363,0.,-0.999898174994542));
#6963=DIRECTION('',(0.,-1.,0.));
#6964=DIRECTION('',(-0.0142702362483363,0.,0.999898174994542));
#6965=DIRECTION('',(0.,-1.,0.));
#6966=DIRECTION('center_axis',(0.104525286015233,0.,-0.994522229305828));
#6967=DIRECTION('ref_axis',(0.994522229305828,0.,0.104525286015233));
#6968=DIRECTION('',(-0.994522229305828,0.,-0.104525286015233));
#6969=DIRECTION('',(0.994522229305828,0.,0.104525286015233));
#6970=DIRECTION('',(0.,-1.,0.));
#6971=DIRECTION('center_axis',(0.115345698196854,0.,0.993325409877086));
#6972=DIRECTION('ref_axis',(-0.993325409877086,0.,0.115345698196854));
#6973=DIRECTION('',(-0.993325409877086,0.,0.115345698196854));
#6974=DIRECTION('',(-0.993325409877086,0.,0.115345698196854));
#6975=DIRECTION('center_axis',(0.,-1.,0.));
#6976=DIRECTION('ref_axis',(1.,0.,0.));
#6977=DIRECTION('center_axis',(0.,-1.,0.));
#6978=DIRECTION('ref_axis',(1.,0.,0.));
#6979=DIRECTION('',(0.,1.,0.));
#6980=DIRECTION('center_axis',(0.,-1.,0.));
#6981=DIRECTION('ref_axis',(1.,0.,0.));
#6982=DIRECTION('center_axis',(0.981014949795783,0.,-0.193932122860493));
#6983=DIRECTION('ref_axis',(0.193932122860493,0.,0.981014949795783));
#6984=DIRECTION('',(-0.193932122860493,0.,-0.981014949795783));
#6985=DIRECTION('',(0.,-1.,0.));
#6986=DIRECTION('',(0.193932122860493,0.,0.981014949795783));
#6987=DIRECTION('',(0.,-1.,0.));
#6988=DIRECTION('center_axis',(-0.104531640519007,0.,-0.994521561420568));
#6989=DIRECTION('ref_axis',(0.994521561420568,0.,-0.104531640519007));
#6990=DIRECTION('',(-0.994521561420568,0.,0.104531640519007));
#6991=DIRECTION('',(0.994521561420568,0.,-0.104531640519007));
#6992=DIRECTION('',(0.,-1.,0.));
#6993=DIRECTION('center_axis',(0.319349083446007,0.,0.947637147278533));
#6994=DIRECTION('ref_axis',(-0.947637147278533,0.,0.319349083446007));
#6995=DIRECTION('',(-0.947637147278533,0.,0.319349083446007));
#6996=DIRECTION('',(-0.947637147278533,0.,0.319349083446007));
#6997=DIRECTION('center_axis',(0.,-1.,0.));
#6998=DIRECTION('ref_axis',(1.,0.,0.));
#6999=DIRECTION('center_axis',(0.,-1.,0.));
#7000=DIRECTION('ref_axis',(1.,0.,0.));
#7001=DIRECTION('',(0.,1.,0.));
#7002=DIRECTION('center_axis',(0.,-1.,0.));
#7003=DIRECTION('ref_axis',(1.,0.,0.));
#7004=DIRECTION('center_axis',(0.817322450628582,0.,-0.576180537417301));
#7005=DIRECTION('ref_axis',(0.576180537417301,0.,0.817322450628582));
#7006=DIRECTION('',(-0.576180537417301,0.,-0.817322450628582));
#7007=DIRECTION('',(0.,-1.,0.));
#7008=DIRECTION('',(0.576180537417301,0.,0.817322450628582));
#7009=DIRECTION('',(0.,-1.,0.));
#7010=DIRECTION('center_axis',(-0.500002766734773,0.,-0.86602380640348));
#7011=DIRECTION('ref_axis',(0.86602380640348,0.,-0.500002766734773));
#7012=DIRECTION('',(-0.86602380640348,0.,0.500002766734773));
#7013=DIRECTION('',(0.86602380640348,0.,-0.500002766734773));
#7014=DIRECTION('',(0.,-1.,0.));
#7015=DIRECTION('center_axis',(0.677178656722426,0.,0.735818637219533));
#7016=DIRECTION('ref_axis',(-0.735818637219533,0.,0.677178656722426));
#7017=DIRECTION('',(-0.735818637219533,0.,0.677178656722426));
#7018=DIRECTION('',(0.,1.,0.));
#7019=DIRECTION('',(-0.735818637219533,0.,0.677178656722426));
#7020=DIRECTION('center_axis',(0.,-1.,0.));
#7021=DIRECTION('ref_axis',(1.,0.,0.));
#7022=DIRECTION('center_axis',(0.,-1.,0.));
#7023=DIRECTION('ref_axis',(1.,0.,0.));
#7024=DIRECTION('',(0.,1.,0.));
#7025=DIRECTION('center_axis',(0.,-1.,0.));
#7026=DIRECTION('ref_axis',(1.,0.,0.));
#7027=DIRECTION('center_axis',(0.,-1.,0.));
#7028=DIRECTION('ref_axis',(1.,0.,0.));
#7029=DIRECTION('center_axis',(0.,-1.,0.));
#7030=DIRECTION('ref_axis',(1.,0.,0.));
#7031=DIRECTION('',(0.,-1.,0.));
#7032=DIRECTION('center_axis',(0.,-1.,0.));
#7033=DIRECTION('ref_axis',(1.,0.,0.));
#7034=DIRECTION('center_axis',(0.919256663858938,0.,-0.393658717610745));
#7035=DIRECTION('ref_axis',(0.393658717610745,0.,0.919256663858937));
#7036=DIRECTION('',(-0.393658717610745,0.,-0.919256663858937));
#7037=DIRECTION('',(0.,-1.,0.));
#7038=DIRECTION('',(0.393658717610745,0.,0.919256663858937));
#7039=DIRECTION('',(0.,-1.,0.));
#7040=DIRECTION('center_axis',(-0.309020032764104,0.,-0.951055529057306));
#7041=DIRECTION('ref_axis',(0.951055529057306,0.,-0.309020032764104));
#7042=DIRECTION('',(-0.951055529057306,0.,0.309020032764104));
#7043=DIRECTION('',(0.951055529057306,0.,-0.309020032764104));
#7044=DIRECTION('center_axis',(0.50939538134165,0.,0.860532594076363));
#7045=DIRECTION('ref_axis',(-0.860532594076363,0.,0.50939538134165));
#7046=DIRECTION('',(-0.860532594076363,0.,0.50939538134165));
#7047=DIRECTION('',(-0.860532594076363,0.,0.50939538134165));
#7048=DIRECTION('center_axis',(0.679667324357505,0.,-0.733520502917751));
#7049=DIRECTION('ref_axis',(0.733520502917751,0.,0.679667324357505));
#7050=DIRECTION('',(-0.733520502917751,0.,-0.679667324357505));
#7051=DIRECTION('',(0.,-1.,0.));
#7052=DIRECTION('',(0.733520502917751,0.,0.679667324357505));
#7053=DIRECTION('',(0.,-1.,0.));
#7054=DIRECTION('center_axis',(-0.669132980519663,0.,-0.743142687766537));
#7055=DIRECTION('ref_axis',(0.743142687766537,0.,-0.669132980519663));
#7056=DIRECTION('',(-0.743142687766537,0.,0.669132980519663));
#7057=DIRECTION('',(0.743142687766537,0.,-0.669132980519663));
#7058=DIRECTION('',(0.,-1.,0.));
#7059=DIRECTION('center_axis',(0.815365975340715,0.,0.578945875066646));
#7060=DIRECTION('ref_axis',(-0.578945875066646,0.,0.815365975340715));
#7061=DIRECTION('',(-0.578945875066646,0.,0.815365975340715));
#7062=DIRECTION('',(-0.578945875066646,0.,0.815365975340715));
#7063=DIRECTION('center_axis',(0.,-1.,0.));
#7064=DIRECTION('ref_axis',(1.,0.,0.));
#7065=DIRECTION('center_axis',(0.,-1.,0.));
#7066=DIRECTION('ref_axis',(1.,0.,0.));
#7067=DIRECTION('',(0.,1.,0.));
#7068=DIRECTION('center_axis',(0.,-1.,0.));
#7069=DIRECTION('ref_axis',(1.,0.,0.));
#7070=DIRECTION('center_axis',(0.32255732989086,0.,-0.94654992944571));
#7071=DIRECTION('ref_axis',(0.94654992944571,0.,0.32255732989086));
#7072=DIRECTION('',(-0.94654992944571,0.,-0.32255732989086));
#7073=DIRECTION('',(0.,-1.,0.));
#7074=DIRECTION('',(0.94654992944571,0.,0.32255732989086));
#7075=DIRECTION('',(0.,-1.,0.));
#7076=DIRECTION('center_axis',(-0.913546757061081,0.,-0.406733724521562));
#7077=DIRECTION('ref_axis',(0.406733724521562,0.,-0.913546757061081));
#7078=DIRECTION('',(-0.406733724521561,0.,0.913546757061082));
#7079=DIRECTION('',(0.406733724521561,0.,-0.913546757061082));
#7080=DIRECTION('',(0.,-1.,0.));
#7081=DIRECTION('center_axis',(0.980352384836028,0.,0.197254154699748));
#7082=DIRECTION('ref_axis',(-0.197254154699748,0.,0.980352384836028));
#7083=DIRECTION('',(-0.197254154699748,0.,0.980352384836028));
#7084=DIRECTION('',(0.,1.,0.));
#7085=DIRECTION('',(-0.197254154699748,0.,0.980352384836028));
#7086=DIRECTION('center_axis',(0.,-1.,0.));
#7087=DIRECTION('ref_axis',(1.,0.,0.));
#7088=DIRECTION('center_axis',(0.,-1.,0.));
#7089=DIRECTION('ref_axis',(1.,0.,0.));
#7090=DIRECTION('',(0.,1.,0.));
#7091=DIRECTION('center_axis',(0.,-1.,0.));
#7092=DIRECTION('ref_axis',(1.,0.,0.));
#7093=DIRECTION('center_axis',(0.,-1.,0.));
#7094=DIRECTION('ref_axis',(1.,0.,0.));
#7095=DIRECTION('center_axis',(0.,-1.,0.));
#7096=DIRECTION('ref_axis',(1.,0.,0.));
#7097=DIRECTION('',(0.,-1.,0.));
#7098=DIRECTION('center_axis',(0.,-1.,0.));
#7099=DIRECTION('ref_axis',(1.,0.,0.));
#7100=DIRECTION('center_axis',(-0.0903257572552624,0.,-0.995912274036355));
#7101=DIRECTION('ref_axis',(0.995912274036355,0.,-0.0903257572552624));
#7102=DIRECTION('',(-0.995912274036355,0.,0.0903257572552624));
#7103=DIRECTION('',(0.,-1.,0.));
#7104=DIRECTION('',(0.995912274036355,0.,-0.0903257572552624));
#7105=DIRECTION('',(0.,-1.,0.));
#7106=DIRECTION('center_axis',(-0.999999999994897,0.,3.19475307855588E-6));
#7107=DIRECTION('ref_axis',(-3.19475307855588E-6,0.,-0.999999999994897));
#7108=DIRECTION('',(3.19475307855588E-6,0.,0.999999999994897));
#7109=DIRECTION('',(-3.19475307855588E-6,0.,-0.999999999994897));
#7110=DIRECTION('',(0.,-1.,0.));
#7111=DIRECTION('center_axis',(0.975826960771375,0.,-0.218544601012476));
#7112=DIRECTION('ref_axis',(0.218544601012476,0.,0.975826960771375));
#7113=DIRECTION('',(0.218544601012476,0.,0.975826960771374));
#7114=DIRECTION('',(0.,1.,0.));
#7115=DIRECTION('',(0.218544601012476,0.,0.975826960771374));
#7116=DIRECTION('center_axis',(0.,-1.,0.));
#7117=DIRECTION('ref_axis',(1.,0.,0.));
#7118=DIRECTION('center_axis',(0.,-1.,0.));
#7119=DIRECTION('ref_axis',(1.,0.,0.));
#7120=DIRECTION('',(0.,1.,0.));
#7121=DIRECTION('center_axis',(0.,-1.,0.));
#7122=DIRECTION('ref_axis',(1.,0.,0.));
#7123=DIRECTION('center_axis',(0.,-1.,0.));
#7124=DIRECTION('ref_axis',(1.,0.,0.));
#7125=DIRECTION('center_axis',(0.,-1.,0.));
#7126=DIRECTION('ref_axis',(1.,0.,0.));
#7127=DIRECTION('',(0.,-1.,0.));
#7128=DIRECTION('center_axis',(0.,-1.,0.));
#7129=DIRECTION('ref_axis',(1.,0.,0.));
#7130=DIRECTION('center_axis',(0.118709882057359,0.,-0.992928982305345));
#7131=DIRECTION('ref_axis',(0.992928982305345,0.,0.118709882057359));
#7132=DIRECTION('',(-0.992928982305345,0.,-0.118709882057359));
#7133=DIRECTION('',(0.,-1.,0.));
#7134=DIRECTION('',(0.992928982305345,0.,0.118709882057359));
#7135=DIRECTION('',(0.,-1.,0.));
#7136=DIRECTION('center_axis',(-0.978148264955328,0.,-0.207908565876639));
#7137=DIRECTION('ref_axis',(0.207908565876639,0.,-0.978148264955328));
#7138=DIRECTION('',(-0.207908565876639,0.,0.978148264955328));
#7139=DIRECTION('',(0.207908565876639,0.,-0.978148264955328));
#7140=DIRECTION('center_axis',(0.999940777925478,0.,-0.0108830437741485));
#7141=DIRECTION('ref_axis',(0.0108830437741485,0.,0.999940777925478));
#7142=DIRECTION('',(0.0108830437741485,0.,0.999940777925478));
#7143=DIRECTION('',(0.0108830437741485,0.,0.999940777925478));
#7144=DIRECTION('center_axis',(0.512307474606336,0.,-0.858802102618804));
#7145=DIRECTION('ref_axis',(0.858802102618804,0.,0.512307474606336));
#7146=DIRECTION('',(-0.858802102618804,0.,-0.512307474606336));
#7147=DIRECTION('',(0.,-1.,0.));
#7148=DIRECTION('',(0.858802102618804,0.,0.512307474606336));
#7149=DIRECTION('',(0.,-1.,0.));
#7150=DIRECTION('center_axis',(-0.809018872199563,0.,-0.58778266767994));
#7151=DIRECTION('ref_axis',(0.58778266767994,0.,-0.809018872199563));
#7152=DIRECTION('',(-0.58778266767994,0.,0.809018872199563));
#7153=DIRECTION('',(0.58778266767994,0.,-0.809018872199563));
#7154=DIRECTION('center_axis',(0.917917888276573,0.,0.396770400082814));
#7155=DIRECTION('ref_axis',(-0.396770400082814,0.,0.917917888276573));
#7156=DIRECTION('',(-0.396770400082814,0.,0.917917888276573));
#7157=DIRECTION('',(-0.396770400082814,0.,0.917917888276573));
#7158=DIRECTION('center_axis',(-0.295413727544757,0.,-0.955369420474673));
#7159=DIRECTION('ref_axis',(0.955369420474673,0.,-0.295413727544757));
#7160=DIRECTION('',(-0.955369420474673,0.,0.295413727544757));
#7161=DIRECTION('',(0.,-1.,0.));
#7162=DIRECTION('',(0.955369420474673,0.,-0.295413727544757));
#7163=DIRECTION('',(0.,-1.,0.));
#7164=DIRECTION('center_axis',(-0.9781469365023,0.,0.207914815756757));
#7165=DIRECTION('ref_axis',(-0.207914815756757,0.,-0.9781469365023));
#7166=DIRECTION('',(0.207914815756757,0.,0.9781469365023));
#7167=DIRECTION('',(-0.207914815756757,0.,-0.9781469365023));
#7168=DIRECTION('',(0.,-1.,0.));
#7169=DIRECTION('center_axis',(0.909064822894285,0.,-0.416654710493212));
#7170=DIRECTION('ref_axis',(0.416654710493212,0.,0.909064822894285));
#7171=DIRECTION('',(0.416654710493212,0.,0.909064822894285));
#7172=DIRECTION('',(0.416654710493212,0.,0.909064822894285));
#7173=DIRECTION('center_axis',(0.,-1.,0.));
#7174=DIRECTION('ref_axis',(1.,0.,0.));
#7175=DIRECTION('center_axis',(0.,-1.,0.));
#7176=DIRECTION('ref_axis',(1.,0.,0.));
#7177=DIRECTION('',(0.,1.,0.));
#7178=DIRECTION('center_axis',(0.,-1.,0.));
#7179=DIRECTION('ref_axis',(1.,0.,0.));
#7180=DIRECTION('center_axis',(-0.487590700388207,0.,-0.87307233886714));
#7181=DIRECTION('ref_axis',(0.87307233886714,0.,-0.487590700388207));
#7182=DIRECTION('',(-0.87307233886714,0.,0.487590700388207));
#7183=DIRECTION('',(0.,-1.,0.));
#7184=DIRECTION('',(0.87307233886714,0.,-0.487590700388207));
#7185=DIRECTION('',(0.,-1.,0.));
#7186=DIRECTION('center_axis',(-0.913544158214796,0.,0.406739561625888));
#7187=DIRECTION('ref_axis',(-0.406739561625888,0.,-0.913544158214796));
#7188=DIRECTION('',(0.406739561625888,0.,0.913544158214796));
#7189=DIRECTION('',(-0.406739561625888,0.,-0.913544158214796));
#7190=DIRECTION('',(0.,-1.,0.));
#7191=DIRECTION('center_axis',(0.802572190079719,0.,-0.596555009794272));
#7192=DIRECTION('ref_axis',(0.596555009794272,0.,0.802572190079719));
#7193=DIRECTION('',(0.596555009794272,0.,0.802572190079719));
#7194=DIRECTION('',(0.596555009794272,0.,0.802572190079719));
#7195=DIRECTION('center_axis',(0.,-1.,0.));
#7196=DIRECTION('ref_axis',(1.,0.,0.));
#7197=DIRECTION('center_axis',(0.,-1.,0.));
#7198=DIRECTION('ref_axis',(1.,0.,0.));
#7199=DIRECTION('',(0.,1.,0.));
#7200=DIRECTION('center_axis',(0.,-1.,0.));
#7201=DIRECTION('ref_axis',(1.,0.,0.));
#7202=DIRECTION('center_axis',(-0.975081051902262,0.,-0.221848917556922));
#7203=DIRECTION('ref_axis',(0.221848917556922,0.,-0.975081051902262));
#7204=DIRECTION('',(-0.221848917556922,0.,0.975081051902262));
#7205=DIRECTION('',(0.,-1.,0.));
#7206=DIRECTION('',(0.221848917556922,0.,-0.975081051902262));
#7207=DIRECTION('',(0.,-1.,0.));
#7208=DIRECTION('center_axis',(-0.309013955982637,0.,0.951057503523294));
#7209=DIRECTION('ref_axis',(-0.951057503523294,0.,-0.309013955982637));
#7210=DIRECTION('',(0.951057503523294,0.,0.309013955982637));
#7211=DIRECTION('',(-0.951057503523294,0.,-0.309013955982637));
#7212=DIRECTION('',(0.,-1.,0.));
#7213=DIRECTION('center_axis',(0.0936988475535703,0.,-0.995600585559858));
#7214=DIRECTION('ref_axis',(0.995600585559858,0.,0.0936988475535703));
#7215=DIRECTION('',(0.995600585559858,0.,0.0936988475535703));
#7216=DIRECTION('',(0.,1.,0.));
#7217=DIRECTION('',(0.995600585559858,0.,0.0936988475535703));
#7218=DIRECTION('center_axis',(0.,-1.,0.));
#7219=DIRECTION('ref_axis',(1.,0.,0.));
#7220=DIRECTION('center_axis',(0.,-1.,0.));
#7221=DIRECTION('ref_axis',(1.,0.,0.));
#7222=DIRECTION('',(0.,1.,0.));
#7223=DIRECTION('center_axis',(0.,-1.,0.));
#7224=DIRECTION('ref_axis',(1.,0.,0.));
#7225=DIRECTION('center_axis',(0.,-1.,0.));
#7226=DIRECTION('ref_axis',(1.,0.,0.));
#7227=DIRECTION('center_axis',(0.,-1.,0.));
#7228=DIRECTION('ref_axis',(1.,0.,0.));
#7229=DIRECTION('',(0.,-1.,0.));
#7230=DIRECTION('center_axis',(0.,-1.,0.));
#7231=DIRECTION('ref_axis',(1.,0.,0.));
#7232=DIRECTION('center_axis',(-0.658457619904923,0.,-0.752617806585218));
#7233=DIRECTION('ref_axis',(0.752617806585218,0.,-0.658457619904923));
#7234=DIRECTION('',(-0.752617806585218,0.,0.658457619904923));
#7235=DIRECTION('',(0.,-1.,0.));
#7236=DIRECTION('',(0.752617806585218,0.,-0.658457619904923));
#7237=DIRECTION('',(0.,-1.,0.));
#7238=DIRECTION('center_axis',(-0.809015116542074,0.,0.587787836899007));
#7239=DIRECTION('ref_axis',(-0.587787836899007,0.,-0.809015116542074));
#7240=DIRECTION('',(0.587787836899007,0.,0.809015116542074));
#7241=DIRECTION('',(-0.587787836899007,0.,-0.809015116542074));
#7242=DIRECTION('',(0.,-1.,0.));
#7243=DIRECTION('center_axis',(0.661003301390021,0.,-0.750382992578785));
#7244=DIRECTION('ref_axis',(0.750382992578785,0.,0.661003301390021));
#7245=DIRECTION('',(0.750382992578785,0.,0.661003301390021));
#7246=DIRECTION('',(0.750382992578785,0.,0.661003301390021));
#7247=DIRECTION('center_axis',(0.,-1.,0.));
#7248=DIRECTION('ref_axis',(1.,0.,0.));
#7249=DIRECTION('center_axis',(0.,-1.,0.));
#7250=DIRECTION('ref_axis',(1.,0.,0.));
#7251=DIRECTION('',(0.,1.,0.));
#7252=DIRECTION('center_axis',(0.,-1.,0.));
#7253=DIRECTION('ref_axis',(1.,0.,0.));
#7254=DIRECTION('center_axis',(-0.800546781801578,0.,-0.5992702646946));
#7255=DIRECTION('ref_axis',(0.5992702646946,0.,-0.800546781801578));
#7256=DIRECTION('',(-0.5992702646946,0.,0.800546781801578));
#7257=DIRECTION('',(0.,-1.,0.));
#7258=DIRECTION('',(0.5992702646946,0.,-0.800546781801578));
#7259=DIRECTION('',(0.,-1.,0.));
#7260=DIRECTION('center_axis',(-0.669128232191225,0.,0.743146963180666));
#7261=DIRECTION('ref_axis',(-0.743146963180666,0.,-0.669128232191225));
#7262=DIRECTION('',(0.743146963180666,0.,0.669128232191225));
#7263=DIRECTION('',(-0.743146963180666,0.,-0.669128232191225));
#7264=DIRECTION('',(0.,-1.,0.));
#7265=DIRECTION('center_axis',(0.490545396583829,0.,-0.871415637850512));
#7266=DIRECTION('ref_axis',(0.871415637850512,0.,0.490545396583829));
#7267=DIRECTION('',(0.871415637850512,0.,0.490545396583829));
#7268=DIRECTION('',(0.871415637850512,0.,0.490545396583829));
#7269=DIRECTION('center_axis',(0.,-1.,0.));
#7270=DIRECTION('ref_axis',(1.,0.,0.));
#7271=DIRECTION('center_axis',(0.,-1.,0.));
#7272=DIRECTION('ref_axis',(1.,0.,0.));
#7273=DIRECTION('',(0.,1.,0.));
#7274=DIRECTION('center_axis',(0.,-1.,0.));
#7275=DIRECTION('ref_axis',(1.,0.,0.));
#7276=DIRECTION('center_axis',(-0.907648207883844,0.,-0.419731736619053));
#7277=DIRECTION('ref_axis',(0.419731736619053,0.,-0.907648207883844));
#7278=DIRECTION('',(-0.419731736619053,0.,0.907648207883844));
#7279=DIRECTION('',(0.,-1.,0.));
#7280=DIRECTION('',(0.419731736619053,0.,-0.907648207883844));
#7281=DIRECTION('',(0.,-1.,0.));
#7282=DIRECTION('center_axis',(-0.499997233260123,0.,0.866027001156559));
#7283=DIRECTION('ref_axis',(-0.866027001156559,0.,-0.499997233260123));
#7284=DIRECTION('',(0.866027001156559,0.,0.499997233260123));
#7285=DIRECTION('',(-0.866027001156559,0.,-0.499997233260123));
#7286=DIRECTION('center_axis',(0.298648304048949,0.,-0.954363238232009));
#7287=DIRECTION('ref_axis',(0.954363238232009,0.,0.298648304048949));
#7288=DIRECTION('',(0.954363238232009,0.,0.298648304048949));
#7289=DIRECTION('',(0.954363238232009,0.,0.298648304048949));
#7290=DIRECTION('center_axis',(-0.981014949795783,0.,0.193932122860492));
#7291=DIRECTION('ref_axis',(-0.193932122860492,0.,-0.981014949795783));
#7292=DIRECTION('',(0.193932122860492,0.,0.981014949795783));
#7293=DIRECTION('',(0.,-1.,0.));
#7294=DIRECTION('',(-0.193932122860492,0.,-0.981014949795783));
#7295=DIRECTION('',(0.,-1.,0.));
#7296=DIRECTION('center_axis',(0.104531640519007,0.,0.994521561420568));
#7297=DIRECTION('ref_axis',(-0.994521561420568,0.,0.104531640519007));
#7298=DIRECTION('',(0.994521561420568,0.,-0.104531640519007));
#7299=DIRECTION('',(-0.994521561420568,0.,0.104531640519007));
#7300=DIRECTION('',(0.,-1.,0.));
#7301=DIRECTION('center_axis',(-0.319349083446007,0.,-0.947637147278533));
#7302=DIRECTION('ref_axis',(0.947637147278533,0.,-0.319349083446007));
#7303=DIRECTION('',(0.947637147278533,0.,-0.319349083446007));
#7304=DIRECTION('',(0.,1.,0.));
#7305=DIRECTION('',(0.947637147278533,0.,-0.319349083446007));
#7306=DIRECTION('center_axis',(0.,-1.,0.));
#7307=DIRECTION('ref_axis',(1.,0.,0.));
#7308=DIRECTION('center_axis',(0.,-1.,0.));
#7309=DIRECTION('ref_axis',(1.,0.,0.));
#7310=DIRECTION('',(0.,1.,0.));
#7311=DIRECTION('center_axis',(0.,-1.,0.));
#7312=DIRECTION('ref_axis',(1.,0.,0.));
#7313=DIRECTION('center_axis',(0.,-1.,0.));
#7314=DIRECTION('ref_axis',(1.,0.,0.));
#7315=DIRECTION('center_axis',(0.,-1.,0.));
#7316=DIRECTION('ref_axis',(1.,0.,0.));
#7317=DIRECTION('',(0.,-1.,0.));
#7318=DIRECTION('center_axis',(0.,-1.,0.));
#7319=DIRECTION('ref_axis',(1.,0.,0.));
#7320=DIRECTION('center_axis',(-0.999898174994542,0.,-0.0142702362483365));
#7321=DIRECTION('ref_axis',(0.0142702362483365,0.,-0.999898174994542));
#7322=DIRECTION('',(-0.0142702362483365,0.,0.999898174994542));
#7323=DIRECTION('',(0.,-1.,0.));
#7324=DIRECTION('',(0.0142702362483365,0.,-0.999898174994542));
#7325=DIRECTION('',(0.,-1.,0.));
#7326=DIRECTION('center_axis',(-0.104525286015233,0.,0.994522229305828));
#7327=DIRECTION('ref_axis',(-0.994522229305828,0.,-0.104525286015233));
#7328=DIRECTION('',(0.994522229305828,0.,0.104525286015233));
#7329=DIRECTION('',(-0.994522229305828,0.,-0.104525286015233));
#7330=DIRECTION('center_axis',(-0.115345698196854,0.,-0.993325409877086));
#7331=DIRECTION('ref_axis',(0.993325409877086,0.,-0.115345698196854));
#7332=DIRECTION('',(0.993325409877086,0.,-0.115345698196854));
#7333=DIRECTION('',(0.993325409877086,0.,-0.115345698196854));
#7334=DIRECTION('center_axis',(0.487590700388207,0.,0.87307233886714));
#7335=DIRECTION('ref_axis',(-0.87307233886714,0.,0.487590700388207));
#7336=DIRECTION('',(0.87307233886714,0.,-0.487590700388207));
#7337=DIRECTION('',(0.,-1.,0.));
#7338=DIRECTION('',(-0.87307233886714,0.,0.487590700388207));
#7339=DIRECTION('',(0.,-1.,0.));
#7340=DIRECTION('center_axis',(0.913544158214796,0.,-0.406739561625888));
#7341=DIRECTION('ref_axis',(0.406739561625888,0.,0.913544158214796));
#7342=DIRECTION('',(-0.406739561625888,0.,-0.913544158214796));
#7343=DIRECTION('',(0.406739561625888,0.,0.913544158214796));
#7344=DIRECTION('',(0.,-1.,0.));
#7345=DIRECTION('center_axis',(-0.802572190079719,0.,0.596555009794272));
#7346=DIRECTION('ref_axis',(-0.596555009794272,0.,-0.802572190079719));
#7347=DIRECTION('',(-0.596555009794272,0.,-0.802572190079719));
#7348=DIRECTION('',(0.,1.,0.));
#7349=DIRECTION('',(-0.596555009794272,0.,-0.802572190079719));
#7350=DIRECTION('center_axis',(0.,-1.,0.));
#7351=DIRECTION('ref_axis',(1.,0.,0.));
#7352=DIRECTION('center_axis',(0.,-1.,0.));
#7353=DIRECTION('ref_axis',(1.,0.,0.));
#7354=DIRECTION('',(0.,1.,0.));
#7355=DIRECTION('center_axis',(0.,-1.,0.));
#7356=DIRECTION('ref_axis',(1.,0.,0.));
#7357=DIRECTION('center_axis',(0.,-1.,0.));
#7358=DIRECTION('ref_axis',(1.,0.,0.));
#7359=DIRECTION('center_axis',(0.,-1.,0.));
#7360=DIRECTION('ref_axis',(1.,0.,0.));
#7361=DIRECTION('',(0.,-1.,0.));
#7362=DIRECTION('center_axis',(0.,-1.,0.));
#7363=DIRECTION('ref_axis',(1.,0.,0.));
#7364=DIRECTION('center_axis',(0.658457619904923,0.,0.752617806585217));
#7365=DIRECTION('ref_axis',(-0.752617806585217,0.,0.658457619904923));
#7366=DIRECTION('',(0.752617806585217,0.,-0.658457619904923));
#7367=DIRECTION('',(0.,-1.,0.));
#7368=DIRECTION('',(-0.752617806585217,0.,0.658457619904923));
#7369=DIRECTION('',(0.,-1.,0.));
#7370=DIRECTION('center_axis',(0.809015116542074,0.,-0.587787836899007));
#7371=DIRECTION('ref_axis',(0.587787836899007,0.,0.809015116542074));
#7372=DIRECTION('',(-0.587787836899007,0.,-0.809015116542074));
#7373=DIRECTION('',(0.587787836899007,0.,0.809015116542074));
#7374=DIRECTION('center_axis',(-0.661003301390021,0.,0.750382992578785));
#7375=DIRECTION('ref_axis',(-0.750382992578785,0.,-0.661003301390021));
#7376=DIRECTION('',(-0.750382992578785,0.,-0.661003301390021));
#7377=DIRECTION('',(-0.750382992578785,0.,-0.661003301390021));
#7378=DIRECTION('center_axis',(-0.32255732989086,0.,0.94654992944571));
#7379=DIRECTION('ref_axis',(-0.94654992944571,0.,-0.32255732989086));
#7380=DIRECTION('',(0.94654992944571,0.,0.32255732989086));
#7381=DIRECTION('',(0.,-1.,0.));
#7382=DIRECTION('',(-0.94654992944571,0.,-0.32255732989086));
#7383=DIRECTION('',(0.,-1.,0.));
#7384=DIRECTION('center_axis',(0.913546757061081,0.,0.406733724521562));
#7385=DIRECTION('ref_axis',(-0.406733724521562,0.,0.913546757061081));
#7386=DIRECTION('',(0.406733724521562,0.,-0.913546757061081));
#7387=DIRECTION('',(-0.406733724521562,0.,0.913546757061081));
#7388=DIRECTION('',(0.,-1.,0.));
#7389=DIRECTION('center_axis',(-0.980352384836028,0.,-0.197254154699748));
#7390=DIRECTION('ref_axis',(0.197254154699748,0.,-0.980352384836028));
#7391=DIRECTION('',(0.197254154699748,0.,-0.980352384836028));
#7392=DIRECTION('',(0.,1.,0.));
#7393=DIRECTION('',(0.197254154699748,0.,-0.980352384836028));
#7394=DIRECTION('center_axis',(0.,-1.,0.));
#7395=DIRECTION('ref_axis',(1.,0.,0.));
#7396=DIRECTION('center_axis',(0.,-1.,0.));
#7397=DIRECTION('ref_axis',(1.,0.,0.));
#7398=DIRECTION('',(0.,1.,0.));
#7399=DIRECTION('center_axis',(0.,-1.,0.));
#7400=DIRECTION('ref_axis',(1.,0.,0.));
#7401=DIRECTION('center_axis',(0.,-1.,0.));
#7402=DIRECTION('ref_axis',(1.,0.,0.));
#7403=DIRECTION('center_axis',(0.,-1.,0.));
#7404=DIRECTION('ref_axis',(1.,0.,0.));
#7405=DIRECTION('',(0.,-1.,0.));
#7406=DIRECTION('center_axis',(0.,-1.,0.));
#7407=DIRECTION('ref_axis',(1.,0.,0.));
#7408=DIRECTION('center_axis',(-0.118709882057359,0.,0.992928982305345));
#7409=DIRECTION('ref_axis',(-0.992928982305345,0.,-0.118709882057359));
#7410=DIRECTION('',(0.992928982305345,0.,0.118709882057359));
#7411=DIRECTION('',(0.,-1.,0.));
#7412=DIRECTION('',(-0.992928982305345,0.,-0.118709882057359));
#7413=DIRECTION('',(0.,-1.,0.));
#7414=DIRECTION('center_axis',(0.978148264955328,0.,0.20790856587664));
#7415=DIRECTION('ref_axis',(-0.20790856587664,0.,0.978148264955328));
#7416=DIRECTION('',(0.20790856587664,0.,-0.978148264955328));
#7417=DIRECTION('',(-0.20790856587664,0.,0.978148264955328));
#7418=DIRECTION('',(0.,-1.,0.));
#7419=DIRECTION('center_axis',(-0.999940777925478,0.,0.0108830437741482));
#7420=DIRECTION('ref_axis',(-0.0108830437741482,0.,-0.999940777925478));
#7421=DIRECTION('',(-0.0108830437741482,0.,-0.999940777925478));
#7422=DIRECTION('',(-0.0108830437741482,0.,-0.999940777925478));
#7423=DIRECTION('center_axis',(0.,-1.,0.));
#7424=DIRECTION('ref_axis',(1.,0.,0.));
#7425=DIRECTION('center_axis',(0.,-1.,0.));
#7426=DIRECTION('ref_axis',(1.,0.,0.));
#7427=DIRECTION('',(0.,1.,0.));
#7428=DIRECTION('center_axis',(0.,-1.,0.));
#7429=DIRECTION('ref_axis',(1.,0.,0.));
#7430=DIRECTION('center_axis',(0.0903257572552622,0.,0.995912274036355));
#7431=DIRECTION('ref_axis',(-0.995912274036355,0.,0.0903257572552622));
#7432=DIRECTION('',(0.995912274036355,0.,-0.0903257572552622));
#7433=DIRECTION('',(0.,-1.,0.));
#7434=DIRECTION('',(-0.995912274036355,0.,0.0903257572552622));
#7435=DIRECTION('',(0.,-1.,0.));
#7436=DIRECTION('center_axis',(0.999999999994897,0.,-3.19475307830608E-6));
#7437=DIRECTION('ref_axis',(3.19475307830608E-6,0.,0.999999999994897));
#7438=DIRECTION('',(-3.19475307830608E-6,0.,-0.999999999994897));
#7439=DIRECTION('',(3.19475307830608E-6,0.,0.999999999994897));
#7440=DIRECTION('',(0.,-1.,0.));
#7441=DIRECTION('center_axis',(-0.975826960771375,0.,0.218544601012476));
#7442=DIRECTION('ref_axis',(-0.218544601012476,0.,-0.975826960771375));
#7443=DIRECTION('',(-0.218544601012476,0.,-0.975826960771374));
#7444=DIRECTION('',(-0.218544601012476,0.,-0.975826960771374));
#7445=DIRECTION('center_axis',(0.,-1.,0.));
#7446=DIRECTION('ref_axis',(1.,0.,0.));
#7447=DIRECTION('center_axis',(0.,-1.,0.));
#7448=DIRECTION('ref_axis',(1.,0.,0.));
#7449=DIRECTION('',(0.,1.,0.));
#7450=DIRECTION('center_axis',(0.,-1.,0.));
#7451=DIRECTION('ref_axis',(1.,0.,0.));
#7452=DIRECTION('center_axis',(-0.512307474606336,0.,0.858802102618804));
#7453=DIRECTION('ref_axis',(-0.858802102618804,0.,-0.512307474606336));
#7454=DIRECTION('',(0.858802102618804,0.,0.512307474606336));
#7455=DIRECTION('',(0.,-1.,0.));
#7456=DIRECTION('',(-0.858802102618804,0.,-0.512307474606336));
#7457=DIRECTION('',(0.,-1.,0.));
#7458=DIRECTION('center_axis',(0.809018872199563,0.,0.58778266767994));
#7459=DIRECTION('ref_axis',(-0.58778266767994,0.,0.809018872199563));
#7460=DIRECTION('',(0.58778266767994,0.,-0.809018872199563));
#7461=DIRECTION('',(-0.58778266767994,0.,0.809018872199563));
#7462=DIRECTION('center_axis',(-0.917917888276573,0.,-0.396770400082814));
#7463=DIRECTION('ref_axis',(0.396770400082814,0.,-0.917917888276573));
#7464=DIRECTION('',(0.396770400082814,0.,-0.917917888276573));
#7465=DIRECTION('',(0.,1.,0.));
#7466=DIRECTION('',(0.396770400082814,0.,-0.917917888276573));
#7467=DIRECTION('center_axis',(0.,-1.,0.));
#7468=DIRECTION('ref_axis',(1.,0.,0.));
#7469=DIRECTION('center_axis',(0.,-1.,0.));
#7470=DIRECTION('ref_axis',(1.,0.,0.));
#7471=DIRECTION('',(0.,-1.,0.));
#7472=DIRECTION('center_axis',(0.,-1.,0.));
#7473=DIRECTION('ref_axis',(1.,0.,0.));
#7474=DIRECTION('center_axis',(-0.817322450628582,0.,0.576180537417301));
#7475=DIRECTION('ref_axis',(-0.576180537417301,0.,-0.817322450628582));
#7476=DIRECTION('',(0.576180537417301,0.,0.817322450628582));
#7477=DIRECTION('',(0.,-1.,0.));
#7478=DIRECTION('',(-0.576180537417301,0.,-0.817322450628582));
#7479=DIRECTION('',(0.,-1.,0.));
#7480=DIRECTION('center_axis',(0.500002766734773,0.,0.86602380640348));
#7481=DIRECTION('ref_axis',(-0.86602380640348,0.,0.500002766734773));
#7482=DIRECTION('',(0.86602380640348,0.,-0.500002766734773));
#7483=DIRECTION('',(-0.86602380640348,0.,0.500002766734773));
#7484=DIRECTION('',(0.,-1.,0.));
#7485=DIRECTION('center_axis',(-0.677178656722426,0.,-0.735818637219533));
#7486=DIRECTION('ref_axis',(0.735818637219533,0.,-0.677178656722426));
#7487=DIRECTION('',(0.735818637219533,0.,-0.677178656722426));
#7488=DIRECTION('',(0.,1.,0.));
#7489=DIRECTION('',(0.735818637219533,0.,-0.677178656722426));
#7490=DIRECTION('center_axis',(0.,-1.,0.));
#7491=DIRECTION('ref_axis',(1.,0.,0.));
#7492=DIRECTION('center_axis',(0.,-1.,0.));
#7493=DIRECTION('ref_axis',(1.,0.,0.));
#7494=DIRECTION('',(0.,1.,0.));
#7495=DIRECTION('center_axis',(0.,-1.,0.));
#7496=DIRECTION('ref_axis',(1.,0.,0.));
#7497=DIRECTION('center_axis',(0.,-1.,0.));
#7498=DIRECTION('ref_axis',(1.,0.,0.));
#7499=DIRECTION('center_axis',(0.,-1.,0.));
#7500=DIRECTION('ref_axis',(1.,0.,0.));
#7501=DIRECTION('',(0.,-1.,0.));
#7502=DIRECTION('center_axis',(0.,-1.,0.));
#7503=DIRECTION('ref_axis',(1.,0.,0.));
#7504=DIRECTION('center_axis',(-0.679667324357505,0.,0.733520502917751));
#7505=DIRECTION('ref_axis',(-0.733520502917751,0.,-0.679667324357505));
#7506=DIRECTION('',(0.733520502917751,0.,0.679667324357505));
#7507=DIRECTION('',(0.,-1.,0.));
#7508=DIRECTION('',(-0.733520502917751,0.,-0.679667324357505));
#7509=DIRECTION('',(0.,-1.,0.));
#7510=DIRECTION('center_axis',(0.669132980519662,0.,0.743142687766537));
#7511=DIRECTION('ref_axis',(-0.743142687766537,0.,0.669132980519662));
#7512=DIRECTION('',(0.743142687766537,0.,-0.669132980519662));
#7513=DIRECTION('',(-0.743142687766537,0.,0.669132980519662));
#7514=DIRECTION('center_axis',(-0.815365975340715,0.,-0.578945875066647));
#7515=DIRECTION('ref_axis',(0.578945875066647,0.,-0.815365975340715));
#7516=DIRECTION('',(0.578945875066647,0.,-0.815365975340715));
#7517=DIRECTION('',(0.578945875066647,0.,-0.815365975340715));
#7518=DIRECTION('center_axis',(-0.919256663858938,0.,0.393658717610745));
#7519=DIRECTION('ref_axis',(-0.393658717610745,0.,-0.919256663858938));
#7520=DIRECTION('',(0.393658717610745,0.,0.919256663858938));
#7521=DIRECTION('',(0.,-1.,0.));
#7522=DIRECTION('',(-0.393658717610745,0.,-0.919256663858938));
#7523=DIRECTION('',(0.,-1.,0.));
#7524=DIRECTION('center_axis',(0.309020032764104,0.,0.951055529057306));
#7525=DIRECTION('ref_axis',(-0.951055529057306,0.,0.309020032764104));
#7526=DIRECTION('',(0.951055529057306,0.,-0.309020032764104));
#7527=DIRECTION('',(-0.951055529057306,0.,0.309020032764104));
#7528=DIRECTION('center_axis',(-0.50939538134165,0.,-0.860532594076364));
#7529=DIRECTION('ref_axis',(0.860532594076364,0.,-0.50939538134165));
#7530=DIRECTION('',(0.860532594076363,0.,-0.50939538134165));
#7531=DIRECTION('',(0.860532594076363,0.,-0.50939538134165));
#7532=DIRECTION('center_axis',(0.295413727544757,0.,0.955369420474673));
#7533=DIRECTION('ref_axis',(-0.955369420474673,0.,0.295413727544757));
#7534=DIRECTION('',(0.955369420474673,0.,-0.295413727544757));
#7535=DIRECTION('',(0.,-1.,0.));
#7536=DIRECTION('',(-0.955369420474673,0.,0.295413727544757));
#7537=DIRECTION('',(0.,-1.,0.));
#7538=DIRECTION('center_axis',(0.9781469365023,0.,-0.207914815756757));
#7539=DIRECTION('ref_axis',(0.207914815756757,0.,0.9781469365023));
#7540=DIRECTION('',(-0.207914815756757,0.,-0.9781469365023));
#7541=DIRECTION('',(0.207914815756757,0.,0.9781469365023));
#7542=DIRECTION('center_axis',(-0.909064822894285,0.,0.416654710493212));
#7543=DIRECTION('ref_axis',(-0.416654710493212,0.,-0.909064822894285));
#7544=DIRECTION('',(-0.416654710493212,0.,-0.909064822894285));
#7545=DIRECTION('',(-0.416654710493212,0.,-0.909064822894285));
#7546=DIRECTION('center_axis',(0.0553951891924081,0.,0.998464507638773));
#7547=DIRECTION('ref_axis',(-0.998464507638773,0.,0.0553951891924081));
#7548=DIRECTION('',(0.998464507638773,0.,-0.0553951891924081));
#7549=DIRECTION('',(0.,1.,0.));
#7550=DIRECTION('',(-0.998464507638773,0.,0.0553951891924081));
#7551=DIRECTION('',(0.,-1.,0.));
#7552=DIRECTION('center_axis',(0.0553951891924081,0.,-0.998464507638773));
#7553=DIRECTION('ref_axis',(0.998464507638773,0.,0.0553951891924081));
#7554=DIRECTION('',(0.998464507638773,0.,0.0553951891924081));
#7555=DIRECTION('',(0.,1.,0.));
#7556=DIRECTION('',(0.998464507638773,0.,0.0553951891924081));
#7557=DIRECTION('',(0.,-1.,0.));
#7558=DIRECTION('center_axis',(0.,-1.,0.));
#7559=DIRECTION('ref_axis',(1.,0.,0.));
#7560=DIRECTION('center_axis',(0.,1.,0.));
#7561=DIRECTION('ref_axis',(1.,0.,0.));
#7562=DIRECTION('',(0.,1.,0.));
#7563=DIRECTION('center_axis',(0.,1.,0.));
#7564=DIRECTION('ref_axis',(1.,0.,0.));
#7565=DIRECTION('center_axis',(0.,-1.,0.));
#7566=DIRECTION('ref_axis',(1.,0.,0.));
#7567=DIRECTION('center_axis',(0.,1.,0.));
#7568=DIRECTION('ref_axis',(1.,0.,0.));
#7569=DIRECTION('',(0.,-1.,0.));
#7570=DIRECTION('center_axis',(0.,1.,0.));
#7571=DIRECTION('ref_axis',(1.,0.,0.));
#7572=DIRECTION('center_axis',(0.,-1.,0.));
#7573=DIRECTION('ref_axis',(1.,0.,0.));
#7574=DIRECTION('center_axis',(0.,-1.,0.));
#7575=DIRECTION('ref_axis',(1.,0.,0.));
#7576=DIRECTION('',(0.,1.,0.));
#7577=DIRECTION('center_axis',(0.,-1.,0.));
#7578=DIRECTION('ref_axis',(1.,0.,0.));
#7579=DIRECTION('center_axis',(0.,-1.,0.));
#7580=DIRECTION('ref_axis',(1.,0.,0.));
#7581=DIRECTION('center_axis',(0.,-1.,0.));
#7582=DIRECTION('ref_axis',(1.,0.,0.));
#7583=DIRECTION('',(0.,-1.,0.));
#7584=DIRECTION('center_axis',(0.,-1.,0.));
#7585=DIRECTION('ref_axis',(1.,0.,0.));
#7586=DIRECTION('center_axis',(0.892393222988503,0.,0.451258612731316));
#7587=DIRECTION('ref_axis',(-0.451258612731316,0.,0.892393222988503));
#7588=DIRECTION('',(0.451258612731316,0.,-0.892393222988503));
#7589=DIRECTION('',(-0.451258612731316,0.,0.892393222988503));
#7590=DIRECTION('center_axis',(-0.836998033796095,0.,-0.547205894907457));
#7591=DIRECTION('ref_axis',(0.547205894907457,0.,-0.836998033796095));
#7592=DIRECTION('',(0.547205894907457,0.,-0.836998033796095));
#7593=DIRECTION('',(0.,1.,0.));
#7594=DIRECTION('',(0.547205894907457,0.,-0.836998033796095));
#7595=DIRECTION('',(0.,-1.,0.));
#7596=DIRECTION('center_axis',(0.,-1.,0.));
#7597=DIRECTION('ref_axis',(1.,0.,0.));
#7598=DIRECTION('center_axis',(0.,1.,0.));
#7599=DIRECTION('ref_axis',(1.,0.,0.));
#7600=DIRECTION('',(0.,-1.,0.));
#7601=DIRECTION('center_axis',(0.,1.,0.));
#7602=DIRECTION('ref_axis',(1.,0.,0.));
#7603=DIRECTION('center_axis',(0.,-1.,0.));
#7604=DIRECTION('ref_axis',(1.,0.,0.));
#7605=DIRECTION('center_axis',(0.,-1.,0.));
#7606=DIRECTION('ref_axis',(1.,0.,0.));
#7607=DIRECTION('',(0.,1.,0.));
#7608=DIRECTION('center_axis',(0.,-1.,0.));
#7609=DIRECTION('ref_axis',(1.,0.,0.));
#7610=DIRECTION('center_axis',(0.836998033796095,0.,-0.547205894907457));
#7611=DIRECTION('ref_axis',(0.547205894907457,0.,0.836998033796095));
#7612=DIRECTION('',(-0.547205894907457,0.,-0.836998033796095));
#7613=DIRECTION('',(0.547205894907457,0.,0.836998033796095));
#7614=DIRECTION('center_axis',(-0.892393222988503,0.,0.451258612731316));
#7615=DIRECTION('ref_axis',(-0.451258612731316,0.,-0.892393222988503));
#7616=DIRECTION('',(-0.451258612731316,0.,-0.892393222988503));
#7617=DIRECTION('',(0.,1.,0.));
#7618=DIRECTION('',(-0.451258612731316,0.,-0.892393222988503));
#7619=DIRECTION('',(0.,-1.,0.));
#7620=DIRECTION('center_axis',(0.,-1.,0.));
#7621=DIRECTION('ref_axis',(1.,0.,0.));
#7622=DIRECTION('center_axis',(0.,1.,0.));
#7623=DIRECTION('ref_axis',(1.,0.,0.));
#7624=DIRECTION('',(0.,-1.,0.));
#7625=DIRECTION('center_axis',(0.,1.,0.));
#7626=DIRECTION('ref_axis',(1.,0.,0.));
#7627=DIRECTION('center_axis',(0.,-1.,0.));
#7628=DIRECTION('ref_axis',(1.,0.,0.));
#7629=DIRECTION('center_axis',(0.,-1.,0.));
#7630=DIRECTION('ref_axis',(1.,0.,0.));
#7631=DIRECTION('',(0.,1.,0.));
#7632=DIRECTION('center_axis',(0.,-1.,0.));
#7633=DIRECTION('ref_axis',(1.,0.,0.));
#7634=DIRECTION('center_axis',(-0.055395189192408,0.,-0.998464507638773));
#7635=DIRECTION('ref_axis',(0.998464507638773,0.,-0.055395189192408));
#7636=DIRECTION('',(-0.998464507638773,0.,0.055395189192408));
#7637=DIRECTION('',(0.998464507638773,0.,-0.055395189192408));
#7638=DIRECTION('center_axis',(-0.0553951891924082,0.,0.998464507638773));
#7639=DIRECTION('ref_axis',(-0.998464507638773,0.,-0.0553951891924082));
#7640=DIRECTION('',(-0.998464507638773,0.,-0.0553951891924082));
#7641=DIRECTION('',(0.,1.,0.));
#7642=DIRECTION('',(-0.998464507638773,0.,-0.0553951891924082));
#7643=DIRECTION('',(0.,-1.,0.));
#7644=DIRECTION('center_axis',(0.,-1.,0.));
#7645=DIRECTION('ref_axis',(1.,0.,0.));
#7646=DIRECTION('center_axis',(0.,1.,0.));
#7647=DIRECTION('ref_axis',(1.,0.,0.));
#7648=DIRECTION('',(0.,-1.,0.));
#7649=DIRECTION('center_axis',(0.,1.,0.));
#7650=DIRECTION('ref_axis',(1.,0.,0.));
#7651=DIRECTION('center_axis',(0.,-1.,0.));
#7652=DIRECTION('ref_axis',(1.,0.,0.));
#7653=DIRECTION('center_axis',(0.,-1.,0.));
#7654=DIRECTION('ref_axis',(1.,0.,0.));
#7655=DIRECTION('',(0.,1.,0.));
#7656=DIRECTION('center_axis',(0.,-1.,0.));
#7657=DIRECTION('ref_axis',(1.,0.,0.));
#7658=DIRECTION('center_axis',(-0.892393222988503,0.,-0.451258612731316));
#7659=DIRECTION('ref_axis',(0.451258612731316,0.,-0.892393222988503));
#7660=DIRECTION('',(-0.451258612731316,0.,0.892393222988503));
#7661=DIRECTION('',(0.451258612731316,0.,-0.892393222988503));
#7662=DIRECTION('center_axis',(0.836998033796095,0.,0.547205894907458));
#7663=DIRECTION('ref_axis',(-0.547205894907458,0.,0.836998033796095));
#7664=DIRECTION('',(-0.547205894907458,0.,0.836998033796095));
#7665=DIRECTION('',(0.,1.,0.));
#7666=DIRECTION('',(-0.547205894907458,0.,0.836998033796095));
#7667=DIRECTION('',(0.,-1.,0.));
#7668=DIRECTION('center_axis',(0.,-1.,0.));
#7669=DIRECTION('ref_axis',(1.,0.,0.));
#7670=DIRECTION('center_axis',(0.,1.,0.));
#7671=DIRECTION('ref_axis',(1.,0.,0.));
#7672=DIRECTION('',(0.,-1.,0.));
#7673=DIRECTION('center_axis',(0.,1.,0.));
#7674=DIRECTION('ref_axis',(1.,0.,0.));
#7675=DIRECTION('center_axis',(0.,-1.,0.));
#7676=DIRECTION('ref_axis',(1.,0.,0.));
#7677=DIRECTION('center_axis',(0.,-1.,0.));
#7678=DIRECTION('ref_axis',(1.,0.,0.));
#7679=DIRECTION('',(0.,1.,0.));
#7680=DIRECTION('center_axis',(0.,-1.,0.));
#7681=DIRECTION('ref_axis',(1.,0.,0.));
#7682=DIRECTION('center_axis',(-0.836998033796096,0.,0.547205894907456));
#7683=DIRECTION('ref_axis',(-0.547205894907456,0.,-0.836998033796096));
#7684=DIRECTION('',(0.547205894907456,0.,0.836998033796096));
#7685=DIRECTION('',(-0.547205894907456,0.,-0.836998033796096));
#7686=DIRECTION('center_axis',(0.892393222988504,0.,-0.451258612731315));
#7687=DIRECTION('ref_axis',(0.451258612731315,0.,0.892393222988504));
#7688=DIRECTION('',(0.451258612731315,0.,0.892393222988504));
#7689=DIRECTION('',(0.451258612731315,0.,0.892393222988504));
#7690=DIRECTION('center_axis',(0.,-1.,0.));
#7691=DIRECTION('ref_axis',(1.,0.,0.));
#7692=DIRECTION('center_axis',(0.,1.,0.));
#7693=DIRECTION('ref_axis',(1.,0.,0.));
#7694=DIRECTION('',(0.,-1.,0.));
#7695=DIRECTION('center_axis',(0.,1.,0.));
#7696=DIRECTION('ref_axis',(1.,0.,0.));
#7697=DIRECTION('center_axis',(0.,-1.,0.));
#7698=DIRECTION('ref_axis',(1.,0.,0.));
#7699=DIRECTION('center_axis',(0.,-1.,0.));
#7700=DIRECTION('ref_axis',(1.,0.,0.));
#7701=DIRECTION('axis',(0.,0.,1.));
#7702=DIRECTION('refdir',(1.,0.,0.));
#7703=DIRECTION('center_axis',(0.,-1.,0.));
#7704=DIRECTION('ref_axis',(1.,0.,0.));
#7705=DIRECTION('center_axis',(0.,1.,0.));
#7706=DIRECTION('ref_axis',(1.,0.,0.));
#7707=DIRECTION('',(0.,-1.,0.));
#7708=DIRECTION('center_axis',(0.,1.,0.));
#7709=DIRECTION('ref_axis',(1.,0.,0.));
#7710=DIRECTION('center_axis',(0.,-1.,0.));
#7711=DIRECTION('ref_axis',(1.,0.,0.));
#7712=DIRECTION('center_axis',(0.,1.,0.));
#7713=DIRECTION('ref_axis',(1.,0.,0.));
#7714=DIRECTION('center_axis',(0.,-1.,0.));
#7715=DIRECTION('ref_axis',(1.,0.,0.));
#7716=DIRECTION('',(0.860147585785704,0.,0.510045224139021));
#7717=DIRECTION('',(-0.510045224139015,0.,0.860147585785708));
#7718=DIRECTION('',(0.860147585785706,0.,0.510045224139018));
#7719=DIRECTION('center_axis',(0.,-1.,0.));
#7720=DIRECTION('ref_axis',(-0.600758197939069,0.,-0.799430789755438));
#7721=DIRECTION('',(0.877406199933791,0.,-0.479748225966229));
#7722=DIRECTION('center_axis',(0.,1.,0.));
#7723=DIRECTION('ref_axis',(0.749053332236673,0.,-0.662509702166796));
#7724=DIRECTION('',(0.429092562599351,0.,-0.903260523172535));
#7725=DIRECTION('center_axis',(0.,-1.,0.));
#7726=DIRECTION('ref_axis',(0.72057468488707,0.,-0.693377331256149));
#7727=DIRECTION('',(-0.877406199933791,0.,0.479748225966229));
#7728=DIRECTION('center_axis',(0.,-1.,0.));
#7729=DIRECTION('ref_axis',(0.943439642400352,0.,-0.331544327575508));
#7730=DIRECTION('',(-0.860147585785706,0.,-0.510045224139018));
#7731=DIRECTION('',(0.510045224139015,0.,-0.860147585785708));
#7732=DIRECTION('',(-0.860147585785706,0.,-0.510045224139018));
#7733=DIRECTION('center_axis',(0.,-1.,0.));
#7734=DIRECTION('ref_axis',(-0.891523131063977,0.,-0.452975172363656));
#7735=DIRECTION('',(0.91803072008761,0.,0.39650926467792));
#7736=DIRECTION('center_axis',(0.,1.,0.));
#7737=DIRECTION('ref_axis',(-0.826791968384381,0.,-0.562507814181351));
#7738=DIRECTION('center_axis',(0.860147585785706,0.,0.510045224139019));
#7739=DIRECTION('ref_axis',(0.510045224139019,0.,-0.860147585785706));
#7740=DIRECTION('',(0.,1.,0.));
#7741=DIRECTION('',(0.,1.,0.));
#7742=DIRECTION('',(-0.510045224139019,0.,0.860147585785705));
#7743=DIRECTION('center_axis',(0.,-1.,0.));
#7744=DIRECTION('ref_axis',(-0.891523131063977,0.,-0.452975172363656));
#7745=DIRECTION('center_axis',(0.,-1.,0.));
#7746=DIRECTION('ref_axis',(-0.891523131063977,0.,-0.452975172363656));
#7747=DIRECTION('',(0.,-1.,0.));
#7748=DIRECTION('',(0.,-1.,0.));
#7749=DIRECTION('center_axis',(0.396509264677948,0.,-0.918030720087598));
#7750=DIRECTION('ref_axis',(0.918030720087598,0.,0.396509264677948));
#7751=DIRECTION('',(0.918030720087598,0.,0.396509264677948));
#7752=DIRECTION('',(0.,-1.,0.));
#7753=DIRECTION('center_axis',(0.,-1.,0.));
#7754=DIRECTION('ref_axis',(-0.893553614971487,0.,-0.448956498083487));
#7755=DIRECTION('center_axis',(0.,-1.,0.));
#7756=DIRECTION('ref_axis',(-0.893553614971487,0.,-0.448956498083487));
#7757=DIRECTION('',(0.,-1.,0.));
#7758=DIRECTION('center_axis',(-0.510045224139018,0.,0.860147585785706));
#7759=DIRECTION('ref_axis',(-0.860147585785706,0.,-0.510045224139018));
#7760=DIRECTION('',(0.,-1.,0.));
#7761=DIRECTION('',(0.860147585785706,0.,0.510045224139018));
#7762=DIRECTION('center_axis',(0.510045224139018,0.,-0.860147585785706));
#7763=DIRECTION('ref_axis',(0.860147585785706,0.,0.510045224139018));
#7764=DIRECTION('',(0.860147585785706,0.,0.510045224139018));
#7765=DIRECTION('center_axis',(0.,-1.,0.));
#7766=DIRECTION('ref_axis',(1.,0.,0.));
#7767=DIRECTION('',(-0.510045224139019,0.,0.860147585785705));
#7768=DIRECTION('',(0.860147585785706,0.,0.510045224139018));
#7769=DIRECTION('center_axis',(0.,-1.,0.));
#7770=DIRECTION('ref_axis',(1.,0.,0.));
#7771=DIRECTION('',(0.877406199933791,0.,-0.479748225966229));
#7772=DIRECTION('center_axis',(0.,-1.,0.));
#7773=DIRECTION('ref_axis',(0.720574684887071,0.,-0.693377331256149));
#7774=DIRECTION('',(0.429092562599351,0.,-0.903260523172535));
#7775=DIRECTION('center_axis',(0.,-1.,0.));
#7776=DIRECTION('ref_axis',(0.749053332236673,0.,-0.662509702166795));
#7777=DIRECTION('',(0.877406199933792,0.,-0.479748225966228));
#7778=DIRECTION('center_axis',(0.,-1.,0.));
#7779=DIRECTION('ref_axis',(1.,0.,0.));
#7780=DIRECTION('',(0.860147585785706,0.,0.510045224139018));
#7781=DIRECTION('center_axis',(0.,1.,0.));
#7782=DIRECTION('ref_axis',(1.,0.,0.));
#7783=DIRECTION('center_axis',(0.860147585785706,0.,0.510045224139019));
#7784=DIRECTION('ref_axis',(0.510045224139019,0.,-0.860147585785706));
#7785=DIRECTION('',(0.,-1.,0.));
#7786=DIRECTION('center_axis',(-0.510045224139018,0.,0.860147585785706));
#7787=DIRECTION('ref_axis',(-0.860147585785706,0.,-0.510045224139018));
#7788=DIRECTION('',(0.,-1.,0.));
#7789=DIRECTION('center_axis',(0.,-1.,0.));
#7790=DIRECTION('ref_axis',(1.,0.,0.));
#7791=DIRECTION('',(0.,-1.,0.));
#7792=DIRECTION('center_axis',(0.,-1.,0.));
#7793=DIRECTION('ref_axis',(-0.0606108082303955,0.,0.998161474875512));
#7794=DIRECTION('',(0.,-1.,0.));
#7795=DIRECTION('center_axis',(0.479748225966229,0.,0.877406199933791));
#7796=DIRECTION('ref_axis',(-0.877406199933791,0.,0.479748225966229));
#7797=DIRECTION('',(0.,-1.,0.));
#7798=DIRECTION('center_axis',(0.,-1.,0.));
#7799=DIRECTION('ref_axis',(0.720574684887071,0.,-0.693377331256149));
#7800=DIRECTION('',(0.,-1.,0.));
#7801=DIRECTION('center_axis',(-0.903260523172535,0.,-0.429092562599351));
#7802=DIRECTION('ref_axis',(0.429092562599351,0.,-0.903260523172535));
#7803=DIRECTION('',(0.,-1.,0.));
#7804=DIRECTION('center_axis',(0.,-1.,0.));
#7805=DIRECTION('ref_axis',(0.749053332236673,0.,-0.662509702166795));
#7806=DIRECTION('',(0.,-1.,0.));
#7807=DIRECTION('center_axis',(-0.479748225966228,0.,-0.877406199933792));
#7808=DIRECTION('ref_axis',(0.877406199933792,0.,-0.479748225966228));
#7809=DIRECTION('',(0.,-1.,0.));
#7810=DIRECTION('center_axis',(0.,-1.,0.));
#7811=DIRECTION('ref_axis',(1.,0.,0.));
#7812=DIRECTION('',(0.,-1.,0.));
#7813=DIRECTION('center_axis',(0.510045224139018,0.,-0.860147585785706));
#7814=DIRECTION('ref_axis',(0.860147585785706,0.,0.510045224139018));
#7815=DIRECTION('axis',(0.,0.,1.));
#7816=DIRECTION('refdir',(1.,0.,0.));
#7817=DIRECTION('center_axis',(-1.,-1.83697019872103E-16,0.));
#7818=DIRECTION('ref_axis',(1.83697019872103E-16,-1.,0.));
#7819=DIRECTION('center_axis',(-1.,-1.83697019872103E-16,0.));
#7820=DIRECTION('ref_axis',(1.83697019872103E-16,-1.,0.));
#7821=DIRECTION('',(-1.,-1.83697019872103E-16,0.));
#7822=DIRECTION('center_axis',(-1.,-1.83697019872103E-16,0.));
#7823=DIRECTION('ref_axis',(1.83697019872103E-16,-1.,0.));
#7824=DIRECTION('center_axis',(-1.,-1.83697019872103E-16,0.));
#7825=DIRECTION('ref_axis',(1.83697019872103E-16,-1.,0.));
#7826=DIRECTION('center_axis',(-1.,-1.83697019872103E-16,0.));
#7827=DIRECTION('ref_axis',(1.83697019872103E-16,-1.,0.));
#7828=DIRECTION('',(-1.,-1.83697019872103E-16,0.));
#7829=DIRECTION('center_axis',(-1.,-1.83697019872103E-16,0.));
#7830=DIRECTION('ref_axis',(1.83697019872103E-16,-1.,0.));
#7831=DIRECTION('center_axis',(-1.,-1.83697019872103E-16,0.));
#7832=DIRECTION('ref_axis',(1.83697019872103E-16,-1.,0.));
#7833=DIRECTION('center_axis',(-1.,-1.83697019872103E-16,0.));
#7834=DIRECTION('ref_axis',(1.83697019872103E-16,-1.,0.));
#7835=DIRECTION('center_axis',(-1.,-1.83697019872103E-16,0.));
#7836=DIRECTION('ref_axis',(1.83697019872103E-16,-1.,0.));
#7837=DIRECTION('',(-1.,-1.83697019872103E-16,0.));
#7838=DIRECTION('center_axis',(-1.,-1.83697019872103E-16,0.));
#7839=DIRECTION('ref_axis',(1.83697019872103E-16,-1.,0.));
#7840=DIRECTION('center_axis',(1.,1.83697019872103E-16,0.));
#7841=DIRECTION('ref_axis',(-1.83697019872103E-16,1.,0.));
#7842=DIRECTION('',(0.707106781186551,-0.707106781186544,-8.6595605623549E-17));
#7843=DIRECTION('center_axis',(-1.,-1.83697019872103E-16,0.));
#7844=DIRECTION('ref_axis',(1.83697019872103E-16,-1.,0.));
#7845=DIRECTION('center_axis',(-1.,-1.83697019872103E-16,0.));
#7846=DIRECTION('ref_axis',(1.85037170770859E-16,-1.,0.));
#7847=DIRECTION('center_axis',(-1.,-1.83697019872103E-16,0.));
#7848=DIRECTION('ref_axis',(1.83697019872103E-16,-1.,0.));
#7849=DIRECTION('center_axis',(2.24963967399279E-32,-1.22464679914735E-16,
-1.));
#7850=DIRECTION('ref_axis',(-1.85037170770859E-16,1.,-1.22464679914735E-16));
#7851=DIRECTION('center_axis',(-1.,-1.83697019872103E-16,0.));
#7852=DIRECTION('ref_axis',(1.83697019872103E-16,-1.,0.));
#7853=DIRECTION('center_axis',(-1.,-1.83697019872103E-16,0.));
#7854=DIRECTION('ref_axis',(1.83697019872103E-16,-1.,0.));
#7855=DIRECTION('center_axis',(-1.,-1.83697019872103E-16,0.));
#7856=DIRECTION('ref_axis',(1.83697019872103E-16,-1.,0.));
#7857=DIRECTION('',(1.,1.83697019872103E-16,0.));
#7858=DIRECTION('center_axis',(-1.,-1.83697019872103E-16,0.));
#7859=DIRECTION('ref_axis',(1.85037170770859E-16,-1.,0.));
#7860=DIRECTION('center_axis',(-1.,-1.83697019872103E-16,0.));
#7861=DIRECTION('ref_axis',(1.83697019872103E-16,-1.,0.));
#7862=DIRECTION('center_axis',(2.24963967399279E-32,-1.22464679914735E-16,
-1.));
#7863=DIRECTION('ref_axis',(-1.85037170770859E-16,1.,-1.22464679914735E-16));
#7864=DIRECTION('center_axis',(-1.,-1.83697019872103E-16,0.));
#7865=DIRECTION('ref_axis',(1.83697019872103E-16,-1.,0.));
#7866=DIRECTION('',(-0.707106781186551,0.707106781186544,-8.6595605623549E-17));
#7867=DIRECTION('center_axis',(-1.,-1.83697019872103E-16,0.));
#7868=DIRECTION('ref_axis',(1.83697019872103E-16,-1.,0.));
#7869=DIRECTION('center_axis',(1.,1.83697019872103E-16,0.));
#7870=DIRECTION('ref_axis',(-1.83697019872103E-16,1.,0.));
#7871=DIRECTION('center_axis',(-1.,-1.83697019872103E-16,0.));
#7872=DIRECTION('ref_axis',(1.83697019872103E-16,-1.,0.));
#7873=DIRECTION('center_axis',(1.,1.83697019872103E-16,0.));
#7874=DIRECTION('ref_axis',(-1.83697019872103E-16,1.,0.));
#7875=DIRECTION('center_axis',(-1.,-1.83697019872103E-16,0.));
#7876=DIRECTION('ref_axis',(1.83697019872103E-16,-1.,0.));
#7877=DIRECTION('center_axis',(1.,1.83697019872103E-16,0.));
#7878=DIRECTION('ref_axis',(-1.83697019872103E-16,1.,0.));
#7879=DIRECTION('center_axis',(-1.,-1.83697019872103E-16,0.));
#7880=DIRECTION('ref_axis',(1.83697019872103E-16,-1.,0.));
#7881=DIRECTION('',(-0.707106781186548,0.707106781186547,8.65956056235493E-17));
#7882=DIRECTION('center_axis',(-1.,-1.83697019872103E-16,0.));
#7883=DIRECTION('ref_axis',(1.83697019872103E-16,-1.,0.));
#7884=DIRECTION('center_axis',(-1.,-1.83697019872103E-16,0.));
#7885=DIRECTION('ref_axis',(1.83697019872103E-16,-1.,0.));
#7886=DIRECTION('center_axis',(-1.,-1.83697019872103E-16,0.));
#7887=DIRECTION('ref_axis',(1.83697019872103E-16,-1.,0.));
#7888=DIRECTION('',(1.,1.83697019872103E-16,0.));
#7889=DIRECTION('center_axis',(-1.,-1.83697019872103E-16,0.));
#7890=DIRECTION('ref_axis',(1.83697019872103E-16,-1.,0.));
#7891=DIRECTION('center_axis',(-1.,-1.83697019872103E-16,0.));
#7892=DIRECTION('ref_axis',(1.96129949112834E-16,-1.,0.));
#7893=DIRECTION('center_axis',(-2.24963967399279E-32,1.22464679914735E-16,
1.));
#7894=DIRECTION('ref_axis',(-1.63441624260695E-16,1.,-1.22464679914735E-16));
#7895=DIRECTION('center_axis',(-1.,-1.83697019872103E-16,0.));
#7896=DIRECTION('ref_axis',(1.83697019872103E-16,-1.,0.));
#7897=DIRECTION('center_axis',(-1.,-1.83697019872103E-16,0.));
#7898=DIRECTION('ref_axis',(1.83697019872103E-16,-1.,0.));
#7899=DIRECTION('center_axis',(-1.,-1.83697019872103E-16,0.));
#7900=DIRECTION('ref_axis',(1.83697019872103E-16,-1.,0.));
#7901=DIRECTION('',(1.,1.83697019872103E-16,0.));
#7902=DIRECTION('center_axis',(-1.,-1.83697019872103E-16,0.));
#7903=DIRECTION('ref_axis',(1.83697019872103E-16,-1.,0.));
#7904=DIRECTION('center_axis',(-1.,-1.83697019872103E-16,0.));
#7905=DIRECTION('ref_axis',(1.96129949112834E-16,-1.,0.));
#7906=DIRECTION('center_axis',(-1.,-1.83697019872103E-16,0.));
#7907=DIRECTION('ref_axis',(1.83697019872103E-16,-1.,0.));
#7908=DIRECTION('center_axis',(-2.24963967399279E-32,1.22464679914735E-16,
1.));
#7909=DIRECTION('ref_axis',(-1.63441624260695E-16,1.,-1.22464679914735E-16));
#7910=DIRECTION('center_axis',(-1.,-1.83697019872103E-16,0.));
#7911=DIRECTION('ref_axis',(1.83697019872103E-16,-1.,0.));
#7912=DIRECTION('center_axis',(-1.,-1.83697019872103E-16,0.));
#7913=DIRECTION('ref_axis',(1.83697019872103E-16,-1.,0.));
#7914=DIRECTION('',(1.,1.83697019872103E-16,0.));
#7915=DIRECTION('center_axis',(-1.,-1.83697019872103E-16,0.));
#7916=DIRECTION('ref_axis',(1.83697019872103E-16,-1.,0.));
#7917=DIRECTION('center_axis',(-1.,-1.83697019872103E-16,0.));
#7918=DIRECTION('ref_axis',(1.83697019872103E-16,-1.,0.));
#7919=DIRECTION('',(0.707106781186548,-0.707106781186547,8.65956056235493E-17));
#7920=DIRECTION('center_axis',(-1.,-1.83697019872103E-16,0.));
#7921=DIRECTION('ref_axis',(1.83697019872103E-16,-1.,0.));
#7922=DIRECTION('center_axis',(-1.,-1.83697019872103E-16,0.));
#7923=DIRECTION('ref_axis',(1.85037170770859E-16,-1.,0.));
#7924=DIRECTION('center_axis',(-1.,-1.83697019872103E-16,0.));
#7925=DIRECTION('ref_axis',(1.83697019872103E-16,-1.,0.));
#7926=DIRECTION('center_axis',(2.24963967399279E-32,-1.22464679914735E-16,
-1.));
#7927=DIRECTION('ref_axis',(-2.31296463463574E-16,1.,-1.22464679914735E-16));
#7928=DIRECTION('center_axis',(-1.,-1.83697019872103E-16,0.));
#7929=DIRECTION('ref_axis',(1.83697019872103E-16,-1.,0.));
#7930=DIRECTION('center_axis',(-1.,-1.83697019872103E-16,0.));
#7931=DIRECTION('ref_axis',(1.83697019872103E-16,-1.,0.));
#7932=DIRECTION('',(-1.,-1.83697019872103E-16,0.));
#7933=DIRECTION('center_axis',(-1.,-1.83697019872103E-16,0.));
#7934=DIRECTION('ref_axis',(1.83697019872103E-16,-1.,0.));
#7935=DIRECTION('center_axis',(-1.,-1.83697019872103E-16,0.));
#7936=DIRECTION('ref_axis',(1.85037170770859E-16,-1.,0.));
#7937=DIRECTION('center_axis',(2.24963967399279E-32,-1.22464679914735E-16,
-1.));
#7938=DIRECTION('ref_axis',(-2.31296463463574E-16,1.,-1.22464679914735E-16));
#7939=DIRECTION('center_axis',(-1.,-1.83697019872103E-16,0.));
#7940=DIRECTION('ref_axis',(1.83697019872103E-16,-1.,0.));
#7941=DIRECTION('center_axis',(-1.,-1.83697019872103E-16,0.));
#7942=DIRECTION('ref_axis',(1.83697019872103E-16,-1.,0.));
#7943=DIRECTION('center_axis',(-1.,-1.83697019872103E-16,0.));
#7944=DIRECTION('ref_axis',(1.83697019872103E-16,-1.,0.));
#7945=DIRECTION('center_axis',(1.,1.83697019872103E-16,0.));
#7946=DIRECTION('ref_axis',(-1.83697019872103E-16,1.,0.));
#7947=DIRECTION('center_axis',(1.,1.83697019872103E-16,0.));
#7948=DIRECTION('ref_axis',(-1.83697019872103E-16,1.,0.));
#7949=DIRECTION('center_axis',(-1.,-1.83697019872103E-16,0.));
#7950=DIRECTION('ref_axis',(1.83697019872103E-16,-1.,0.));
#7951=DIRECTION('center_axis',(-1.,-1.83697019872103E-16,0.));
#7952=DIRECTION('ref_axis',(1.83697019872103E-16,-1.,0.));
#7953=DIRECTION('',(-1.,-1.83697019872103E-16,0.));
#7954=DIRECTION('center_axis',(-1.,-1.83697019872103E-16,0.));
#7955=DIRECTION('ref_axis',(1.83697019872103E-16,-1.,0.));
#7956=DIRECTION('center_axis',(-1.,-1.83697019872103E-16,0.));
#7957=DIRECTION('ref_axis',(1.57361694361665E-16,-1.,0.));
#7958=DIRECTION('center_axis',(-1.,-1.83697019872103E-16,0.));
#7959=DIRECTION('ref_axis',(1.83697019872103E-16,-1.,0.));
#7960=DIRECTION('center_axis',(2.24963967399279E-32,-1.22464679914735E-16,
-1.));
#7961=DIRECTION('ref_axis',(-1.96702117952081E-16,1.,-1.22464679914735E-16));
#7962=DIRECTION('center_axis',(-1.,-1.83697019872103E-16,0.));
#7963=DIRECTION('ref_axis',(1.83697019872103E-16,-1.,0.));
#7964=DIRECTION('center_axis',(-1.,-1.83697019872103E-16,0.));
#7965=DIRECTION('ref_axis',(1.83697019872103E-16,-1.,0.));
#7966=DIRECTION('center_axis',(-1.,-1.83697019872103E-16,0.));
#7967=DIRECTION('ref_axis',(1.83697019872103E-16,-1.,0.));
#7968=DIRECTION('',(0.866025403784443,-0.499999999999992,6.12323399573667E-17));
#7969=DIRECTION('center_axis',(-1.,-1.83697019872103E-16,0.));
#7970=DIRECTION('ref_axis',(2.01689087919369E-16,-1.,0.));
#7971=DIRECTION('center_axis',(-1.,-1.83697019872103E-16,0.));
#7972=DIRECTION('ref_axis',(1.83697019872103E-16,-1.,0.));
#7973=DIRECTION('center_axis',(-2.24963967399279E-32,1.22464679914735E-16,
1.));
#7974=DIRECTION('ref_axis',(-1.89083519924408E-16,1.,-1.22464679914735E-16));
#7975=DIRECTION('center_axis',(-1.,-1.83697019872103E-16,0.));
#7976=DIRECTION('ref_axis',(1.88974131851091E-16,-1.,0.));
#7977=DIRECTION('center_axis',(-1.,-1.83697019872103E-16,0.));
#7978=DIRECTION('ref_axis',(1.83697019872103E-16,-1.,0.));
#7979=DIRECTION('center_axis',(-2.24963967399279E-32,1.22464679914735E-16,
1.));
#7980=DIRECTION('ref_axis',(-1.77163248610397E-16,1.,-1.22464679914735E-16));
#7981=DIRECTION('center_axis',(-1.,-1.83697019872103E-16,0.));
#7982=DIRECTION('ref_axis',(1.83697019872103E-16,-1.,0.));
#7983=DIRECTION('center_axis',(-1.,-1.83697019872103E-16,0.));
#7984=DIRECTION('ref_axis',(1.83697019872103E-16,-1.,0.));
#7985=DIRECTION('center_axis',(-1.,-1.83697019872103E-16,0.));
#7986=DIRECTION('ref_axis',(1.83697019872103E-16,-1.,0.));
#7987=DIRECTION('',(-0.500000000000007,0.866025403784435,-1.0605752387249E-16));
#7988=DIRECTION('center_axis',(-1.,-1.83697019872103E-16,0.));
#7989=DIRECTION('ref_axis',(1.91801449774277E-16,-1.,0.));
#7990=DIRECTION('center_axis',(-1.,-1.83697019872103E-16,0.));
#7991=DIRECTION('ref_axis',(1.83697019872103E-16,-1.,0.));
#7992=DIRECTION('center_axis',(-2.24963967399279E-32,1.22464679914735E-16,
1.));
#7993=DIRECTION('ref_axis',(-1.79813859163385E-16,1.,-1.22464679914735E-16));
#7994=DIRECTION('center_axis',(-1.,-1.83697019872103E-16,0.));
#7995=DIRECTION('ref_axis',(1.87747066251861E-16,-1.,0.));
#7996=DIRECTION('center_axis',(-1.,-1.83697019872103E-16,0.));
#7997=DIRECTION('ref_axis',(1.83697019872103E-16,-1.,0.));
#7998=DIRECTION('center_axis',(2.24963967399279E-32,-1.22464679914735E-16,
-1.));
#7999=DIRECTION('ref_axis',(-1.7601287461112E-16,1.,-1.22464679914735E-16));
#8000=DIRECTION('center_axis',(-1.,-1.83697019872103E-16,0.));
#8001=DIRECTION('ref_axis',(1.83697019872103E-16,-1.,0.));
#8002=DIRECTION('center_axis',(-1.,-1.83697019872103E-16,0.));
#8003=DIRECTION('ref_axis',(1.83697019872103E-16,-1.,0.));
#8004=DIRECTION('center_axis',(-1.,-1.83697019872103E-16,0.));
#8005=DIRECTION('ref_axis',(1.83697019872103E-16,-1.,0.));
#8006=DIRECTION('',(0.500000000000007,-0.866025403784435,1.0605752387249E-16));
#8007=DIRECTION('center_axis',(-1.,-1.83697019872103E-16,0.));
#8008=DIRECTION('ref_axis',(1.85037170770859E-16,-1.,0.));
#8009=DIRECTION('center_axis',(-1.,-1.83697019872103E-16,0.));
#8010=DIRECTION('ref_axis',(1.83697019872103E-16,-1.,0.));
#8011=DIRECTION('center_axis',(2.24963967399279E-32,-1.22464679914735E-16,
-1.));
#8012=DIRECTION('ref_axis',(-1.73472347597681E-16,1.,-1.22464679914735E-16));
#8013=DIRECTION('center_axis',(-1.,-1.83697019872103E-16,0.));
#8014=DIRECTION('ref_axis',(1.97210791246963E-16,-1.,0.));
#8015=DIRECTION('center_axis',(-1.,-1.83697019872103E-16,0.));
#8016=DIRECTION('ref_axis',(1.83697019872103E-16,-1.,0.));
#8017=DIRECTION('center_axis',(2.24963967399279E-32,-1.22464679914735E-16,
-1.));
#8018=DIRECTION('ref_axis',(-1.84885116794028E-16,1.,-1.22464679914735E-16));
#8019=DIRECTION('center_axis',(-1.,-1.83697019872103E-16,0.));
#8020=DIRECTION('ref_axis',(1.83697019872103E-16,-1.,0.));
#8021=DIRECTION('center_axis',(-1.,-1.83697019872103E-16,0.));
#8022=DIRECTION('ref_axis',(1.83697019872103E-16,-1.,0.));
#8023=DIRECTION('center_axis',(-1.,-1.83697019872103E-16,0.));
#8024=DIRECTION('ref_axis',(1.83697019872103E-16,-1.,0.));
#8025=DIRECTION('',(-0.866025403784443,0.499999999999992,-6.12323399573667E-17));
#8026=DIRECTION('center_axis',(1.,1.83697019872103E-16,0.));
#8027=DIRECTION('ref_axis',(-1.83697019872103E-16,1.,0.));
#8028=DIRECTION('center_axis',(1.,1.83697019872103E-16,0.));
#8029=DIRECTION('ref_axis',(-1.83697019872103E-16,1.,0.));
#8030=DIRECTION('center_axis',(-1.,-1.83697019872103E-16,0.));
#8031=DIRECTION('ref_axis',(1.83697019872103E-16,-1.,0.));
#8032=DIRECTION('center_axis',(1.,1.83697019872103E-16,0.));
#8033=DIRECTION('ref_axis',(-1.83697019872103E-16,1.,0.));
#8034=DIRECTION('center_axis',(1.,1.83697019872103E-16,0.));
#8035=DIRECTION('ref_axis',(-1.83697019872103E-16,1.,0.));
#8036=DIRECTION('center_axis',(1.,-1.83697019872103E-16,0.));
#8037=DIRECTION('ref_axis',(-1.83697019872103E-16,-1.,0.));
#8038=DIRECTION('center_axis',(-1.,1.83697019872103E-16,0.));
#8039=DIRECTION('ref_axis',(-1.83697019872103E-16,-1.,0.));
#8040=DIRECTION('',(1.,-1.83697019872103E-16,0.));
#8041=DIRECTION('center_axis',(-1.,1.83697019872103E-16,0.));
#8042=DIRECTION('ref_axis',(-1.83697019872103E-16,-1.,0.));
#8043=DIRECTION('center_axis',(1.,-1.83697019872103E-16,0.));
#8044=DIRECTION('ref_axis',(-1.57361694361665E-16,-1.,0.));
#8045=DIRECTION('center_axis',(-1.,1.83697019872103E-16,0.));
#8046=DIRECTION('ref_axis',(-1.83697019872103E-16,-1.,0.));
#8047=DIRECTION('center_axis',(-2.24963967399279E-32,-1.22464679914735E-16,
1.));
#8048=DIRECTION('ref_axis',(1.96702117952081E-16,1.,1.22464679914735E-16));
#8049=DIRECTION('center_axis',(-1.,1.83697019872103E-16,0.));
#8050=DIRECTION('ref_axis',(-1.83697019872103E-16,-1.,0.));
#8051=DIRECTION('center_axis',(1.,-1.83697019872103E-16,0.));
#8052=DIRECTION('ref_axis',(-1.83697019872103E-16,-1.,0.));
#8053=DIRECTION('center_axis',(-1.,1.83697019872103E-16,0.));
#8054=DIRECTION('ref_axis',(-1.83697019872103E-16,-1.,0.));
#8055=DIRECTION('',(-0.866025403784443,-0.499999999999992,-6.12323399573667E-17));
#8056=DIRECTION('center_axis',(1.,-1.83697019872103E-16,0.));
#8057=DIRECTION('ref_axis',(-2.01689087919369E-16,-1.,0.));
#8058=DIRECTION('center_axis',(-1.,1.83697019872103E-16,0.));
#8059=DIRECTION('ref_axis',(-1.83697019872103E-16,-1.,0.));
#8060=DIRECTION('center_axis',(2.24963967399279E-32,1.22464679914735E-16,
-1.));
#8061=DIRECTION('ref_axis',(1.89083519924408E-16,1.,1.22464679914735E-16));
#8062=DIRECTION('center_axis',(1.,-1.83697019872103E-16,0.));
#8063=DIRECTION('ref_axis',(-1.88974131851091E-16,-1.,0.));
#8064=DIRECTION('center_axis',(-1.,1.83697019872103E-16,0.));
#8065=DIRECTION('ref_axis',(-1.83697019872103E-16,-1.,0.));
#8066=DIRECTION('center_axis',(2.24963967399279E-32,1.22464679914735E-16,
-1.));
#8067=DIRECTION('ref_axis',(1.77163248610397E-16,1.,1.22464679914735E-16));
#8068=DIRECTION('center_axis',(-1.,1.83697019872103E-16,0.));
#8069=DIRECTION('ref_axis',(-1.83697019872103E-16,-1.,0.));
#8070=DIRECTION('center_axis',(1.,-1.83697019872103E-16,0.));
#8071=DIRECTION('ref_axis',(-1.83697019872103E-16,-1.,0.));
#8072=DIRECTION('center_axis',(-1.,1.83697019872103E-16,0.));
#8073=DIRECTION('ref_axis',(-1.83697019872103E-16,-1.,0.));
#8074=DIRECTION('',(0.500000000000007,0.866025403784435,1.0605752387249E-16));
#8075=DIRECTION('center_axis',(1.,-1.83697019872103E-16,0.));
#8076=DIRECTION('ref_axis',(-1.91801449774277E-16,-1.,0.));
#8077=DIRECTION('center_axis',(-1.,1.83697019872103E-16,0.));
#8078=DIRECTION('ref_axis',(-1.83697019872103E-16,-1.,0.));
#8079=DIRECTION('center_axis',(2.24963967399279E-32,1.22464679914735E-16,
-1.));
#8080=DIRECTION('ref_axis',(1.79813859163385E-16,1.,1.22464679914735E-16));
#8081=DIRECTION('center_axis',(1.,-1.83697019872103E-16,0.));
#8082=DIRECTION('ref_axis',(-1.87747066251861E-16,-1.,0.));
#8083=DIRECTION('center_axis',(-1.,1.83697019872103E-16,0.));
#8084=DIRECTION('ref_axis',(-1.83697019872103E-16,-1.,0.));
#8085=DIRECTION('center_axis',(-2.24963967399279E-32,-1.22464679914735E-16,
1.));
#8086=DIRECTION('ref_axis',(1.7601287461112E-16,1.,1.22464679914735E-16));
#8087=DIRECTION('center_axis',(-1.,1.83697019872103E-16,0.));
#8088=DIRECTION('ref_axis',(-1.83697019872103E-16,-1.,0.));
#8089=DIRECTION('center_axis',(1.,-1.83697019872103E-16,0.));
#8090=DIRECTION('ref_axis',(-1.83697019872103E-16,-1.,0.));
#8091=DIRECTION('center_axis',(-1.,1.83697019872103E-16,0.));
#8092=DIRECTION('ref_axis',(-1.83697019872103E-16,-1.,0.));
#8093=DIRECTION('',(-0.500000000000007,-0.866025403784435,-1.0605752387249E-16));
#8094=DIRECTION('center_axis',(1.,-1.83697019872103E-16,0.));
#8095=DIRECTION('ref_axis',(-1.85037170770859E-16,-1.,0.));
#8096=DIRECTION('center_axis',(-1.,1.83697019872103E-16,0.));
#8097=DIRECTION('ref_axis',(-1.83697019872103E-16,-1.,0.));
#8098=DIRECTION('center_axis',(-2.24963967399279E-32,-1.22464679914735E-16,
1.));
#8099=DIRECTION('ref_axis',(1.73472347597681E-16,1.,1.22464679914735E-16));
#8100=DIRECTION('center_axis',(1.,-1.83697019872103E-16,0.));
#8101=DIRECTION('ref_axis',(-1.97210791246963E-16,-1.,0.));
#8102=DIRECTION('center_axis',(-1.,1.83697019872103E-16,0.));
#8103=DIRECTION('ref_axis',(-1.83697019872103E-16,-1.,0.));
#8104=DIRECTION('center_axis',(-2.24963967399279E-32,-1.22464679914735E-16,
1.));
#8105=DIRECTION('ref_axis',(1.84885116794028E-16,1.,1.22464679914735E-16));
#8106=DIRECTION('center_axis',(-1.,1.83697019872103E-16,0.));
#8107=DIRECTION('ref_axis',(-1.83697019872103E-16,-1.,0.));
#8108=DIRECTION('center_axis',(1.,-1.83697019872103E-16,0.));
#8109=DIRECTION('ref_axis',(-1.83697019872103E-16,-1.,0.));
#8110=DIRECTION('center_axis',(-1.,1.83697019872103E-16,0.));
#8111=DIRECTION('ref_axis',(-1.83697019872103E-16,-1.,0.));
#8112=DIRECTION('',(0.866025403784443,0.499999999999992,6.12323399573667E-17));
#8113=DIRECTION('center_axis',(-1.,1.83697019872103E-16,0.));
#8114=DIRECTION('ref_axis',(1.83697019872103E-16,1.,0.));
#8115=DIRECTION('center_axis',(-1.,1.83697019872103E-16,0.));
#8116=DIRECTION('ref_axis',(1.83697019872103E-16,1.,0.));
#8117=DIRECTION('center_axis',(1.,-1.83697019872103E-16,0.));
#8118=DIRECTION('ref_axis',(-1.83697019872103E-16,-1.,0.));
#8119=DIRECTION('center_axis',(-1.,1.83697019872103E-16,0.));
#8120=DIRECTION('ref_axis',(1.83697019872103E-16,1.,0.));
#8121=DIRECTION('center_axis',(-1.,1.83697019872103E-16,0.));
#8122=DIRECTION('ref_axis',(1.83697019872103E-16,1.,0.));
#8123=DIRECTION('',(7.70371977754894E-34,-4.27642353614751E-50,1.));
#8124=DIRECTION('',(-8.32667268468866E-17,-1.,2.13821176807375E-50));
#8125=DIRECTION('',(-2.2034386889519E-17,-1.,-2.578956115478E-50));
#8126=DIRECTION('',(7.70371977754894E-34,-4.27642353614753E-50,1.));
#8127=DIRECTION('',(0.,0.,1.));
#8128=DIRECTION('',(1.,0.,0.));
#8129=DIRECTION('',(0.,0.,1.));
#8130=DIRECTION('',(1.,0.,0.));
#8131=DIRECTION('',(0.,0.,1.));
#8132=DIRECTION('',(1.,0.,0.));
#8133=DIRECTION('',(0.,0.,1.));
#8134=DIRECTION('',(1.,0.,0.));
#8135=DIRECTION('',(0.,0.,1.));
#8136=DIRECTION('',(1.,0.,0.));
#8137=DIRECTION('',(0.087155742747658,7.46523770068995E-17,-0.996194698091746));
#8138=DIRECTION('',(-2.17224899799281E-16,1.,5.59328207912988E-17));
#8139=CARTESIAN_POINT('',(0.,0.,0.));
#8140=CARTESIAN_POINT('',(0.,0.,0.));
#8141=CARTESIAN_POINT('Origin',(-1.8,0.,0.));
#8142=CARTESIAN_POINT('',(-1.7,4.8,-5.8783046359073E-16));
#8143=CARTESIAN_POINT('Origin',(-1.7,1.83697019872105E-17,0.));
#8144=CARTESIAN_POINT('',(-1.955,4.8,-5.8783046359073E-16));
#8145=CARTESIAN_POINT('',(-1.8,4.8,-5.87830463590729E-16));
#8146=CARTESIAN_POINT('Origin',(-1.955,-2.84730380801758E-17,0.));
#8147=CARTESIAN_POINT('Origin',(-1.8,0.,0.));
#8148=CARTESIAN_POINT('',(1.7,4.872,-5.96647920544591E-16));
#8149=CARTESIAN_POINT('Origin',(1.7,6.42939569552361E-16,0.));
#8150=CARTESIAN_POINT('',(-1.7,4.872,-5.96647920544591E-16));
#8151=CARTESIAN_POINT('',(-1.8,4.872,-5.96647920544591E-16));
#8152=CARTESIAN_POINT('Origin',(-1.7,1.83697019872105E-17,0.));
#8153=CARTESIAN_POINT('Origin',(-1.8,0.,0.));
#8154=CARTESIAN_POINT('',(1.955,-4.8,5.90585918888811E-16));
#8155=CARTESIAN_POINT('',(1.955,4.8,-5.87830463590729E-16));
#8156=CARTESIAN_POINT('Origin',(1.955,6.89782309619747E-16,0.));
#8157=CARTESIAN_POINT('Origin',(1.955,6.89782309619747E-16,0.));
#8158=CARTESIAN_POINT('',(1.7,4.8,-5.87830463590729E-16));
#8159=CARTESIAN_POINT('',(-1.8,4.8,-5.87830463590729E-16));
#8160=CARTESIAN_POINT('Origin',(1.7,6.42939569552361E-16,0.));
#8161=CARTESIAN_POINT('Origin',(1.955,6.89782309619747E-16,0.));
#8162=CARTESIAN_POINT('',(2.,-4.845,-5.93341374186893E-16));
#8163=CARTESIAN_POINT('',(1.955,-4.8,-5.87830463590729E-16));
#8164=CARTESIAN_POINT('Origin',(2.,6.98048675513991E-16,0.));
#8165=CARTESIAN_POINT('Origin',(1.8,8.67361737988404E-16,0.));
#8166=CARTESIAN_POINT('',(1.8,6.,-7.34788079488412E-16));
#8167=CARTESIAN_POINT('Origin',(1.8,6.61309271539571E-16,0.));
#8168=CARTESIAN_POINT('',(2.,5.8,-7.10295143505465E-16));
#8169=CARTESIAN_POINT('Origin',(1.8,5.8,-7.10295143505465E-16));
#8170=CARTESIAN_POINT('Origin',(2.,6.98048675513991E-16,0.));
#8171=CARTESIAN_POINT('Origin',(-1.8,0.,0.));
#8172=CARTESIAN_POINT('',(-1.8,6.,-7.34788079488412E-16));
#8173=CARTESIAN_POINT('Origin',(-1.8,2.02467570659351E-31,0.));
#8174=CARTESIAN_POINT('',(-1.8,6.,-7.34788079488412E-16));
#8175=CARTESIAN_POINT('Origin',(-1.8,0.,0.));
#8176=CARTESIAN_POINT('',(-2.,5.8,-7.10295143505465E-16));
#8177=CARTESIAN_POINT('Origin',(-2.,-3.67394039744204E-17,0.));
#8178=CARTESIAN_POINT('Origin',(-1.8,5.8,-7.10295143505465E-16));
#8179=CARTESIAN_POINT('Origin',(-2.,-3.67394039744204E-17,0.));
#8180=CARTESIAN_POINT('',(-2.,4.845,-5.93341374186893E-16));
#8181=CARTESIAN_POINT('',(-2.,4.845,-5.93341374186893E-16));
#8182=CARTESIAN_POINT('Origin',(-2.,-3.67394039744204E-17,0.));
#8183=CARTESIAN_POINT('Origin',(-2.,5.8,0.));
#8184=CARTESIAN_POINT('Origin',(2.,5.8,0.));
#8185=CARTESIAN_POINT('Origin',(1.7,4.8,0.));
#8186=CARTESIAN_POINT('Origin',(-1.7,4.8,0.));
#8187=CARTESIAN_POINT('Origin',(-1.955,-2.84730380801757E-17,0.));
#8188=CARTESIAN_POINT('',(-1.955,3.1184375,3.81898450271607E-16));
#8189=CARTESIAN_POINT('',(-1.955,-3.1184375,-3.81898450271607E-16));
#8190=CARTESIAN_POINT('Origin',(-1.955,-2.84730380801757E-17,0.));
#8191=CARTESIAN_POINT('',(-2.,-3.0734375,-3.76387539675444E-16));
#8192=CARTESIAN_POINT('',(-1.955,-3.1184375,-3.81898450271607E-16));
#8193=CARTESIAN_POINT('Origin',(-2.,-3.67394039744204E-17,0.));
#8194=CARTESIAN_POINT('Origin',(-1.955,-2.84730380801757E-17,0.));
#8195=CARTESIAN_POINT('Origin',(-1.8,0.,0.));
#8196=CARTESIAN_POINT('',(-1.7890625,3.1184375,-3.81898450271607E-16));
#8197=CARTESIAN_POINT('',(-1.8,3.1184375,-3.81898450271607E-16));
#8198=CARTESIAN_POINT('Origin',(-1.7890625,2.00918615485137E-18,0.));
#8199=CARTESIAN_POINT('Origin',(-1.7890625,0.,0.));
#8200=CARTESIAN_POINT('',(-1.6625,3.2,-3.91886975727153E-16));
#8201=CARTESIAN_POINT('Origin',(-1.7890625,3.25741379310345,-3.98918137522258E-16));
#8202=CARTESIAN_POINT('Origin',(-1.6625,2.52583402324144E-17,0.));
#8203=CARTESIAN_POINT('Origin',(-1.8,0.,0.));
#8204=CARTESIAN_POINT('',(-1.6625,3.272,-4.00704432681014E-16));
#8205=CARTESIAN_POINT('Origin',(-1.6625,2.52583402324144E-17,0.));
#8206=CARTESIAN_POINT('',(1.6625,3.272,-4.00704432681014E-16));
#8207=CARTESIAN_POINT('',(-1.8,3.272,-4.00704432681014E-16));
#8208=CARTESIAN_POINT('Origin',(1.6625,6.36050931307157E-16,0.));
#8209=CARTESIAN_POINT('Origin',(1.7890625,8.67361737988404E-16,0.));
#8210=CARTESIAN_POINT('',(1.6625,3.2,-3.91886975727153E-16));
#8211=CARTESIAN_POINT('Origin',(1.6625,6.36050931307157E-16,0.));
#8212=CARTESIAN_POINT('',(1.7890625,3.1184375,-3.81898450271607E-16));
#8213=CARTESIAN_POINT('Origin',(1.7890625,3.25741379310345,-3.98918137522258E-16));
#8214=CARTESIAN_POINT('Origin',(1.7890625,6.5930008538472E-16,0.));
#8215=CARTESIAN_POINT('Origin',(-1.8,0.,0.));
#8216=CARTESIAN_POINT('',(1.955,3.1184375,-3.81898450271607E-16));
#8217=CARTESIAN_POINT('',(-1.8,3.1184375,-3.81898450271607E-16));
#8218=CARTESIAN_POINT('Origin',(1.955,6.89782309619747E-16,0.));
#8219=CARTESIAN_POINT('Origin',(2.,6.98048675513991E-16,0.));
#8220=CARTESIAN_POINT('',(2.,3.0734375,-3.76387539675444E-16));
#8221=CARTESIAN_POINT('',(2.,3.0734375,-3.76387539675444E-16));
#8222=CARTESIAN_POINT('Origin',(2.,6.98048675513991E-16,0.));
#8223=CARTESIAN_POINT('Origin',(1.8,8.67361737988404E-16,0.));
#8224=CARTESIAN_POINT('',(2.,2.2,-2.69422295812418E-16));
#8225=CARTESIAN_POINT('Origin',(2.,6.98048675513991E-16,0.));
#8226=CARTESIAN_POINT('',(1.8,2.,-2.44929359829471E-16));
#8227=CARTESIAN_POINT('Origin',(1.8,2.2,-2.69422295812418E-16));
#8228=CARTESIAN_POINT('Origin',(1.8,6.61309271539571E-16,0.));
#8229=CARTESIAN_POINT('Origin',(-1.8,0.,0.));
#8230=CARTESIAN_POINT('',(-1.8,2.,-2.44929359829471E-16));
#8231=CARTESIAN_POINT('',(-1.8,2.,-2.44929359829471E-16));
#8232=CARTESIAN_POINT('Origin',(-1.8,1.86988015034452E-31,0.));
#8233=CARTESIAN_POINT('Origin',(-1.8,0.,0.));
#8234=CARTESIAN_POINT('',(-2.,2.2,-2.69422295812418E-16));
#8235=CARTESIAN_POINT('Origin',(-1.8,2.2,-2.69422295812418E-16));
#8236=CARTESIAN_POINT('Origin',(-2.,-3.67394039744205E-17,0.));
#8237=CARTESIAN_POINT('Origin',(2.,2.2,0.));
#8238=CARTESIAN_POINT('Origin',(1.6625,3.272,0.));
#8239=CARTESIAN_POINT('Origin',(-1.6625,3.2,0.));
#8240=CARTESIAN_POINT('Origin',(-2.,2.2,0.));
#8241=CARTESIAN_POINT('Origin',(-1.8,0.,0.));
#8242=CARTESIAN_POINT('',(1.95,3.2,-3.91886975727153E-16));
#8243=CARTESIAN_POINT('Origin',(1.95,6.88863824520387E-16,0.));
#8244=CARTESIAN_POINT('',(1.85,3.2,-3.91886975727153E-16));
#8245=CARTESIAN_POINT('',(-1.8,3.2,-3.91886975727153E-16));
#8246=CARTESIAN_POINT('Origin',(1.85,6.70494122533176E-16,0.));
#8247=CARTESIAN_POINT('Origin',(1.86,8.67361737988404E-16,0.));
#8248=CARTESIAN_POINT('',(1.905,4.22108058265378,-5.16933282449E-16));
#8249=CARTESIAN_POINT('Origin',(1.905,6.80597458626142E-16,0.));
#8250=CARTESIAN_POINT('',(1.95,4.14313829631318,-5.07388105300476E-16));
#8251=CARTESIAN_POINT('Origin',(1.86,4.14313829631318,-5.07388105300475E-16));
#8252=CARTESIAN_POINT('Origin',(1.95,6.88863824520387E-16,0.));
#8253=CARTESIAN_POINT('Origin',(1.65333333333334,6.34367041958329E-16,0.));
#8254=CARTESIAN_POINT('',(1.65333333333334,4.36638040039984,-5.3472737812094E-16));
#8255=CARTESIAN_POINT('Origin',(1.65333333333334,6.34367041958329E-16,0.));
#8256=CARTESIAN_POINT('',(1.65333333333334,4.36638040039984,-5.3472737812094E-16));
#8257=CARTESIAN_POINT('Origin',(1.66333333333334,8.67361737988404E-16,0.));
#8258=CARTESIAN_POINT('',(1.64333333333333,4.38370090847553,-5.3684852859839E-16));
#8259=CARTESIAN_POINT('Origin',(1.64333333333334,6.32530071759608E-16,0.));
#8260=CARTESIAN_POINT('Origin',(1.66333333333334,4.38370090847553,-5.3684852859839E-16));
#8261=CARTESIAN_POINT('Origin',(1.76333333333333,8.67361737988404E-16,0.));
#8262=CARTESIAN_POINT('',(1.86725638178747,4.64,-5.68236114804372E-16));
#8263=CARTESIAN_POINT('Origin',(1.86725638178747,6.73664068441309E-16,0.));
#8264=CARTESIAN_POINT('',(1.64333333333333,4.58,-5.60888234009488E-16));
#8265=CARTESIAN_POINT('Origin',(1.76333333333333,4.58,-5.60888234009488E-16));
#8266=CARTESIAN_POINT('Origin',(1.64333333333334,6.32530071759608E-16,0.));
#8267=CARTESIAN_POINT('Origin',(1.90725638178747,6.81011949236193E-16,0.));
#8268=CARTESIAN_POINT('',(1.90725638178747,4.57071796769724,-5.59751512894572E-16));
#8269=CARTESIAN_POINT('Origin',(1.90725638178747,6.81011949236193E-16,0.));
#8270=CARTESIAN_POINT('',(1.90725638178747,4.57071796769724,-5.59751512894572E-16));
#8271=CARTESIAN_POINT('Origin',(1.80333333333334,8.67361737988404E-16,0.));
#8272=CARTESIAN_POINT('',(1.80333333333334,4.39071796769724,-5.3770787050992E-16));
#8273=CARTESIAN_POINT('Origin',(1.80333333333334,6.61921594939145E-16,0.));
#8274=CARTESIAN_POINT('Origin',(1.80333333333334,4.51071796769724,-5.52403632099688E-16));
#8275=CARTESIAN_POINT('Origin',(1.80333333333334,8.67361737988404E-16,0.));
#8276=CARTESIAN_POINT('',(1.99385892216591,4.62071796769724,-5.65874746890309E-16));
#8277=CARTESIAN_POINT('Origin',(1.99385892216591,6.96920577817067E-16,0.));
#8278=CARTESIAN_POINT('',(1.80333333333334,4.29071796769724,-5.25461402518447E-16));
#8279=CARTESIAN_POINT('Origin',(1.80333333333334,4.51071796769724,-5.52403632099688E-16));
#8280=CARTESIAN_POINT('Origin',(1.80333333333334,6.61921594939145E-16,0.));
#8281=CARTESIAN_POINT('Origin',(1.99385892216591,6.96920577817067E-16,0.));
#8282=CARTESIAN_POINT('',(1.95385892216591,4.69,-5.74359348800109E-16));
#8283=CARTESIAN_POINT('Origin',(1.95385892216591,6.89572697022182E-16,0.));
#8284=CARTESIAN_POINT('',(1.99385892216591,4.62071796769724,-5.65874746890309E-16));
#8285=CARTESIAN_POINT('Origin',(1.76333333333333,8.67361737988404E-16,0.));
#8286=CARTESIAN_POINT('',(1.54333333333334,4.58,-5.60888234009488E-16));
#8287=CARTESIAN_POINT('Origin',(1.54333333333334,6.14160369772398E-16,0.));
#8288=CARTESIAN_POINT('Origin',(1.76333333333333,4.58,-5.60888234009488E-16));
#8289=CARTESIAN_POINT('Origin',(1.66333333333334,8.67361737988404E-16,0.));
#8290=CARTESIAN_POINT('',(1.60333333333334,4.27977786002139,-5.24121625733691E-16));
#8291=CARTESIAN_POINT('Origin',(1.60333333333334,6.25182190964724E-16,0.));
#8292=CARTESIAN_POINT('',(1.54333333333333,4.38370090847553,-5.3684852859839E-16));
#8293=CARTESIAN_POINT('Origin',(1.66333333333334,4.38370090847553,-5.3684852859839E-16));
#8294=CARTESIAN_POINT('Origin',(1.54333333333334,6.14160369772398E-16,0.));
#8295=CARTESIAN_POINT('Origin',(1.60333333333334,6.25182190964724E-16,0.));
#8296=CARTESIAN_POINT('',(1.85,4.13736479362129,-5.06681055141326E-16));
#8297=CARTESIAN_POINT('Origin',(1.85,6.70494122533176E-16,0.));
#8298=CARTESIAN_POINT('',(1.60333333333334,4.27977786002139,-5.2412162573369E-16));
#8299=CARTESIAN_POINT('Origin',(1.85,4.14313829631318,0.));
#8300=CARTESIAN_POINT('Origin',(1.54333333333334,4.58,0.));
#8301=CARTESIAN_POINT('Origin',(1.80333333333334,4.29071796769724,0.));
#8302=CARTESIAN_POINT('Origin',(1.64333333333334,4.58,0.));
#8303=CARTESIAN_POINT('Origin',(1.95,4.14313829631318,0.));
#8304=CARTESIAN_POINT('Origin',(1.8,0.,0.));
#8305=CARTESIAN_POINT('',(-1.95,3.2,3.91886975727153E-16));
#8306=CARTESIAN_POINT('Origin',(-1.95,6.88863824520387E-16,0.));
#8307=CARTESIAN_POINT('',(-1.85,3.2,3.91886975727153E-16));
#8308=CARTESIAN_POINT('',(1.8,3.2,3.91886975727153E-16));
#8309=CARTESIAN_POINT('Origin',(-1.85,6.70494122533176E-16,0.));
#8310=CARTESIAN_POINT('Origin',(-1.86,8.67361737988404E-16,0.));
#8311=CARTESIAN_POINT('',(-1.905,4.22108058265378,5.16933282449E-16));
#8312=CARTESIAN_POINT('Origin',(-1.905,6.80597458626142E-16,0.));
#8313=CARTESIAN_POINT('',(-1.95,4.14313829631318,5.07388105300476E-16));
#8314=CARTESIAN_POINT('Origin',(-1.86,4.14313829631318,5.07388105300475E-16));
#8315=CARTESIAN_POINT('Origin',(-1.95,6.88863824520387E-16,0.));
#8316=CARTESIAN_POINT('Origin',(-1.65333333333334,6.34367041958329E-16,
0.));
#8317=CARTESIAN_POINT('',(-1.65333333333334,4.36638040039984,5.3472737812094E-16));
#8318=CARTESIAN_POINT('Origin',(-1.65333333333334,6.34367041958329E-16,
0.));
#8319=CARTESIAN_POINT('',(-1.65333333333334,4.36638040039984,5.3472737812094E-16));
#8320=CARTESIAN_POINT('Origin',(-1.66333333333334,8.67361737988404E-16,
0.));
#8321=CARTESIAN_POINT('',(-1.64333333333333,4.38370090847553,5.3684852859839E-16));
#8322=CARTESIAN_POINT('Origin',(-1.64333333333334,6.32530071759608E-16,
0.));
#8323=CARTESIAN_POINT('Origin',(-1.66333333333334,4.38370090847553,5.3684852859839E-16));
#8324=CARTESIAN_POINT('Origin',(-1.76333333333333,8.67361737988404E-16,
0.));
#8325=CARTESIAN_POINT('',(-1.86725638178747,4.64,5.68236114804372E-16));
#8326=CARTESIAN_POINT('Origin',(-1.86725638178747,6.73664068441309E-16,
0.));
#8327=CARTESIAN_POINT('',(-1.64333333333333,4.58,5.60888234009488E-16));
#8328=CARTESIAN_POINT('Origin',(-1.76333333333333,4.58,5.60888234009488E-16));
#8329=CARTESIAN_POINT('Origin',(-1.64333333333334,6.32530071759608E-16,
0.));
#8330=CARTESIAN_POINT('Origin',(-1.90725638178747,6.81011949236193E-16,
0.));
#8331=CARTESIAN_POINT('',(-1.90725638178747,4.57071796769724,5.59751512894572E-16));
#8332=CARTESIAN_POINT('Origin',(-1.90725638178747,6.81011949236193E-16,
0.));
#8333=CARTESIAN_POINT('',(-1.90725638178747,4.57071796769724,5.59751512894572E-16));
#8334=CARTESIAN_POINT('Origin',(-1.80333333333334,8.67361737988404E-16,
0.));
#8335=CARTESIAN_POINT('',(-1.80333333333334,4.39071796769724,5.3770787050992E-16));
#8336=CARTESIAN_POINT('Origin',(-1.80333333333334,6.61921594939145E-16,
0.));
#8337=CARTESIAN_POINT('Origin',(-1.80333333333334,4.51071796769724,5.52403632099688E-16));
#8338=CARTESIAN_POINT('Origin',(-1.80333333333334,8.67361737988404E-16,
0.));
#8339=CARTESIAN_POINT('',(-1.99385892216591,4.62071796769724,5.65874746890309E-16));
#8340=CARTESIAN_POINT('Origin',(-1.99385892216591,6.96920577817067E-16,
0.));
#8341=CARTESIAN_POINT('',(-1.80333333333334,4.29071796769724,5.25461402518447E-16));
#8342=CARTESIAN_POINT('Origin',(-1.80333333333334,4.51071796769724,5.52403632099688E-16));
#8343=CARTESIAN_POINT('Origin',(-1.80333333333334,6.61921594939145E-16,
0.));
#8344=CARTESIAN_POINT('Origin',(-1.99385892216591,6.96920577817067E-16,
0.));
#8345=CARTESIAN_POINT('',(-1.95385892216591,4.69,5.74359348800109E-16));
#8346=CARTESIAN_POINT('Origin',(-1.95385892216591,6.89572697022182E-16,
0.));
#8347=CARTESIAN_POINT('',(-1.99385892216591,4.62071796769724,5.65874746890309E-16));
#8348=CARTESIAN_POINT('Origin',(-1.76333333333333,8.67361737988404E-16,
0.));
#8349=CARTESIAN_POINT('',(-1.54333333333334,4.58,5.60888234009488E-16));
#8350=CARTESIAN_POINT('Origin',(-1.54333333333334,6.14160369772398E-16,
0.));
#8351=CARTESIAN_POINT('Origin',(-1.76333333333333,4.58,5.60888234009488E-16));
#8352=CARTESIAN_POINT('Origin',(-1.66333333333334,8.67361737988404E-16,
0.));
#8353=CARTESIAN_POINT('',(-1.60333333333334,4.27977786002139,5.24121625733691E-16));
#8354=CARTESIAN_POINT('Origin',(-1.60333333333334,6.25182190964724E-16,
0.));
#8355=CARTESIAN_POINT('',(-1.54333333333333,4.38370090847553,5.3684852859839E-16));
#8356=CARTESIAN_POINT('Origin',(-1.66333333333334,4.38370090847553,5.3684852859839E-16));
#8357=CARTESIAN_POINT('Origin',(-1.54333333333334,6.14160369772398E-16,
0.));
#8358=CARTESIAN_POINT('Origin',(-1.60333333333334,6.25182190964724E-16,
0.));
#8359=CARTESIAN_POINT('',(-1.85,4.13736479362129,5.06681055141326E-16));
#8360=CARTESIAN_POINT('Origin',(-1.85,6.70494122533176E-16,0.));
#8361=CARTESIAN_POINT('',(-1.60333333333334,4.27977786002139,5.2412162573369E-16));
#8362=CARTESIAN_POINT('Origin',(-1.85,4.14313829631318,0.));
#8363=CARTESIAN_POINT('Origin',(-1.54333333333334,4.58,0.));
#8364=CARTESIAN_POINT('Origin',(-1.80333333333334,4.29071796769724,0.));
#8365=CARTESIAN_POINT('Origin',(-1.64333333333334,4.58,0.));
#8366=CARTESIAN_POINT('Origin',(-1.95,4.14313829631318,0.));
#8367=CARTESIAN_POINT('',(0.,0.,0.));
#8368=CARTESIAN_POINT('Origin',(0.,0.,-5.78529249999847));
#8369=CARTESIAN_POINT('',(1.954,2.39295984553393E-16,-5.64925672970459));
#8370=CARTESIAN_POINT('Origin',(6.92117815378051E-16,0.,-5.64925672970459));
#8371=CARTESIAN_POINT('',(1.570585,-1.92341189303885E-16,-5.99999999999847));
#8372=CARTESIAN_POINT('',(1.8052925,2.21084568164972E-16,-5.78529249999847));
#8373=CARTESIAN_POINT('Origin',(0.,0.,-5.99999999999847));
#8374=CARTESIAN_POINT('Origin',(-3.95474398665704,0.6,2.4));
#8375=CARTESIAN_POINT('',(-3.86963751125752,0.6,0.96));
#8376=CARTESIAN_POINT('',(-2.24510552006891,0.6,2.4));
#8377=CARTESIAN_POINT('Ctrl Pts',(-3.86963751125752,0.6,0.96));
#8378=CARTESIAN_POINT('Ctrl Pts',(-3.85395158312663,0.6,1.11423006273542));
#8379=CARTESIAN_POINT('Ctrl Pts',(-3.81170536802524,0.6,1.27490216957991));
#8380=CARTESIAN_POINT('Ctrl Pts',(-3.67998890871741,0.6,1.59107732632764));
#8381=CARTESIAN_POINT('Ctrl Pts',(-3.54752952367749,0.6,1.78769245274213));
#8382=CARTESIAN_POINT('Ctrl Pts',(-3.26545084874928,0.6,2.06770924479005));
#8383=CARTESIAN_POINT('Ctrl Pts',(-3.06525849356145,0.6,2.19987575347413));
#8384=CARTESIAN_POINT('Ctrl Pts',(-2.69093530578108,0.6,2.35339781620156));
#8385=CARTESIAN_POINT('Ctrl Pts',(-2.44978343309361,0.6,2.39999999999952));
#8386=CARTESIAN_POINT('Ctrl Pts',(-2.24510552006891,0.6,2.39999999999952));
#8387=CARTESIAN_POINT('',(3.86963751125752,0.600000000000001,0.96));
#8388=CARTESIAN_POINT('',(-4.,0.6,0.96));
#8389=CARTESIAN_POINT('',(2.24510552006891,0.6,2.4));
#8390=CARTESIAN_POINT('Ctrl Pts',(2.24510552006891,0.600000000000001,2.39999999999952));
#8391=CARTESIAN_POINT('Ctrl Pts',(2.44978343309361,0.600000000000001,2.39999999999952));
#8392=CARTESIAN_POINT('Ctrl Pts',(2.69093530578108,0.600000000000001,2.35339781620157));
#8393=CARTESIAN_POINT('Ctrl Pts',(3.06525849356145,0.600000000000001,2.19987575347413));
#8394=CARTESIAN_POINT('Ctrl Pts',(3.26545084874928,0.600000000000001,2.06770924479005));
#8395=CARTESIAN_POINT('Ctrl Pts',(3.54752952367749,0.600000000000001,1.78769245274213));
#8396=CARTESIAN_POINT('Ctrl Pts',(3.67998890871741,0.600000000000001,1.59107732632764));
#8397=CARTESIAN_POINT('Ctrl Pts',(3.81170536802524,0.600000000000001,1.27490216957991));
#8398=CARTESIAN_POINT('Ctrl Pts',(3.85395158312663,0.600000000000001,1.11423006273542));
#8399=CARTESIAN_POINT('Ctrl Pts',(3.86963751125752,0.600000000000001,0.96));
#8400=CARTESIAN_POINT('',(-3.87238559709742,0.6,2.39999999999952));
#8401=CARTESIAN_POINT('Origin',(3.95474398665704,-0.6,2.4));
#8402=CARTESIAN_POINT('',(-2.24510552006891,-0.600000000000001,2.4));
#8403=CARTESIAN_POINT('',(-3.86963751125752,-0.600000000000001,0.96));
#8404=CARTESIAN_POINT('Ctrl Pts',(-2.24510552006891,-0.600000000000001,
2.39999999999952));
#8405=CARTESIAN_POINT('Ctrl Pts',(-2.44978343309361,-0.600000000000001,
2.39999999999952));
#8406=CARTESIAN_POINT('Ctrl Pts',(-2.69093530578108,-0.600000000000001,
2.35339781620156));
#8407=CARTESIAN_POINT('Ctrl Pts',(-3.06525849356145,-0.600000000000001,
2.19987575347413));
#8408=CARTESIAN_POINT('Ctrl Pts',(-3.26545084874928,-0.600000000000001,
2.06770924479005));
#8409=CARTESIAN_POINT('Ctrl Pts',(-3.54752952367749,-0.600000000000001,
1.78769245274213));
#8410=CARTESIAN_POINT('Ctrl Pts',(-3.67998890871741,-0.600000000000001,
1.59107732632764));
#8411=CARTESIAN_POINT('Ctrl Pts',(-3.81170536802524,-0.600000000000001,
1.27490216957991));
#8412=CARTESIAN_POINT('Ctrl Pts',(-3.85395158312663,-0.600000000000001,
1.11423006273542));
#8413=CARTESIAN_POINT('Ctrl Pts',(-3.86963751125752,-0.600000000000001,
0.96));
#8414=CARTESIAN_POINT('',(2.24510552006891,-0.6,2.4));
#8415=CARTESIAN_POINT('',(0.0823583895596134,-0.6,2.39999999999952));
#8416=CARTESIAN_POINT('',(3.86963751125752,-0.6,0.96));
#8417=CARTESIAN_POINT('Ctrl Pts',(3.86963751125752,-0.6,0.96));
#8418=CARTESIAN_POINT('Ctrl Pts',(3.85395158312663,-0.6,1.11423006273542));
#8419=CARTESIAN_POINT('Ctrl Pts',(3.81170536802524,-0.6,1.27490216957991));
#8420=CARTESIAN_POINT('Ctrl Pts',(3.67998890871741,-0.6,1.59107732632764));
#8421=CARTESIAN_POINT('Ctrl Pts',(3.54752952367749,-0.6,1.78769245274213));
#8422=CARTESIAN_POINT('Ctrl Pts',(3.26545084874928,-0.6,2.06770924479005));
#8423=CARTESIAN_POINT('Ctrl Pts',(3.06525849356145,-0.6,2.19987575347413));
#8424=CARTESIAN_POINT('Ctrl Pts',(2.69093530578108,-0.6,2.35339781620157));
#8425=CARTESIAN_POINT('Ctrl Pts',(2.44978343309361,-0.6,2.39999999999952));
#8426=CARTESIAN_POINT('Ctrl Pts',(2.24510552006891,-0.6,2.39999999999952));
#8427=CARTESIAN_POINT('',(4.,-0.6,0.96));
#8428=CARTESIAN_POINT('Origin',(0.,0.,0.96));
#8429=CARTESIAN_POINT('Origin',(-1.0781306403225E-16,0.,0.96));
#8430=CARTESIAN_POINT('',(3.91587722848039,-4.79556651371252E-16,0.96));
#8431=CARTESIAN_POINT('Origin',(-1.0781306403225E-16,0.,0.96));
#8432=CARTESIAN_POINT('Origin',(-1.0781306403225E-16,0.,0.96));
#8433=CARTESIAN_POINT('Origin',(-3.79002720753781,0.,2.39999999999952));
#8434=CARTESIAN_POINT('Origin',(-2.94035629178425E-16,0.,2.39999999999952));
#8435=CARTESIAN_POINT('Origin',(-3.79002720753781,0.,2.39999999999952));
#8436=CARTESIAN_POINT('Origin',(-2.94035629178425E-16,0.,2.39999999999952));
#8437=CARTESIAN_POINT('Origin',(-9.80118763929471E-17,0.,0.799999999999521));
#8438=CARTESIAN_POINT('',(3.91780884605665,-4.79793206299446E-16,0.939449188395684));
#8439=CARTESIAN_POINT('Origin',(0.,-2.39896603149723E-16,0.939449188395683));
#8440=CARTESIAN_POINT('Origin',(2.32389732910985,-2.84595342564146E-16,
0.799999999999521));
#8441=CARTESIAN_POINT('Origin',(-1.4701781458924E-16,0.,1.1999999999989));
#8442=CARTESIAN_POINT('',(4.,-4.89858719658941E-16,-1.72986625024407E-12));
#8443=CARTESIAN_POINT('Origin',(-5.48504848161485E-29,0.,-1.72917236085368E-12));
#8444=CARTESIAN_POINT('',(3.8950136037689,-4.77001594249098E-16,1.1999999999989));
#8445=CARTESIAN_POINT('Origin',(8.32667268468867E-16,0.,-5.99999999999847));
#8446=CARTESIAN_POINT('Origin',(-1.78524999999977,0.,-7.71874504793049E-13));
#8447=CARTESIAN_POINT('',(1.78525000000062,-2.18630069817857E-16,-7.71535613175445E-13));
#8448=CARTESIAN_POINT('Origin',(-1.72131914709554E-28,0.,-7.71605002114484E-13));
#8449=CARTESIAN_POINT('Origin',(6.4320293882545E-17,0.,-0.525000000000627));
#8450=CARTESIAN_POINT('',(1.78525000000062,-2.18630069817857E-16,-1.05000000000048));
#8451=CARTESIAN_POINT('Origin',(1.28640587765262E-16,0.,-1.05000000000048));
#8452=CARTESIAN_POINT('',(1.78525000000062,-2.18630069817857E-16,-0.525000000000627));
#8453=CARTESIAN_POINT('Origin',(1.51425770758387E-16,0.,-1.23597895546358));
#8454=CARTESIAN_POINT('',(1.954,-2.39295984553393E-16,-1.34228357377612));
#8455=CARTESIAN_POINT('Origin',(1.64449664645919E-16,0.,-1.34228357377612));
#8456=CARTESIAN_POINT('',(1.89262500000135,-2.31779714823791E-16,-1.23597895546358));
#8457=CARTESIAN_POINT('Origin',(4.54650013348477E-16,0.,-3.71097895546402));
#8458=CARTESIAN_POINT('',(1.954,-2.39295984553393E-16,-3.71097895546402));
#8459=CARTESIAN_POINT('',(0.,0.,0.));
#8460=CARTESIAN_POINT('Origin',(3.44895709521403E-16,0.,86.8));
#8461=CARTESIAN_POINT('',(-2.,0.,86.8));
#8462=CARTESIAN_POINT('Origin',(3.44895709521403E-16,0.,86.8));
#8463=CARTESIAN_POINT('',(-2.,2.,86.8));
#8464=CARTESIAN_POINT('',(-2.,0.,86.8));
#8465=CARTESIAN_POINT('Origin',(3.44895709521403E-16,2.,86.8));
#8466=CARTESIAN_POINT('Origin',(5.11429163215176E-16,0.,42.));
#8467=CARTESIAN_POINT('',(-2.,0.,42.));
#8468=CARTESIAN_POINT('Origin',(5.11429163215176E-16,0.,42.));
#8469=CARTESIAN_POINT('',(-2.,2.,42.));
#8470=CARTESIAN_POINT('',(-2.,0.,42.));
#8471=CARTESIAN_POINT('Origin',(5.11429163215176E-16,2.,42.));
#8472=CARTESIAN_POINT('Origin',(5.11429163215176E-16,0.,42.));
#8473=CARTESIAN_POINT('',(-6.00000000000001,0.,42.));
#8474=CARTESIAN_POINT('Origin',(5.11429163215176E-16,0.,42.));
#8475=CARTESIAN_POINT('',(-6.00000000000001,-1.,42.));
#8476=CARTESIAN_POINT('',(-6.00000000000001,0.,42.));
#8477=CARTESIAN_POINT('Origin',(5.11429163215176E-16,-1.,42.));
#8478=CARTESIAN_POINT('Origin',(5.11429163215176E-16,0.,42.));
#8479=CARTESIAN_POINT('',(-7.00000000000001,-1.,42.));
#8480=CARTESIAN_POINT('Origin',(5.11429163215176E-16,-1.,42.));
#8481=CARTESIAN_POINT('',(-7.00000000000001,0.,42.));
#8482=CARTESIAN_POINT('',(-7.00000000000001,0.,42.));
#8483=CARTESIAN_POINT('Origin',(5.11429163215176E-16,0.,42.));
#8484=CARTESIAN_POINT('Origin',(0.,-1.,42.));
#8485=CARTESIAN_POINT('Origin',(0.,0.,50.));
#8486=CARTESIAN_POINT('',(35.,0.,100.));
#8487=CARTESIAN_POINT('',(35.,0.,0.));
#8488=CARTESIAN_POINT('',(35.,0.,100.));
#8489=CARTESIAN_POINT('',(-35.,0.,100.));
#8490=CARTESIAN_POINT('',(-35.,0.,100.));
#8491=CARTESIAN_POINT('',(-35.,0.,0.));
#8492=CARTESIAN_POINT('',(-35.,0.,0.));
#8493=CARTESIAN_POINT('',(35.,0.,0.));
#8494=CARTESIAN_POINT('',(-7.00000000000001,0.,86.8));
#8495=CARTESIAN_POINT('Origin',(5.11429163215176E-16,0.,86.8));
#8496=CARTESIAN_POINT('Origin',(5.11429163215176E-16,0.,86.8));
#8497=CARTESIAN_POINT('',(-6.00000000000001,0.,86.8));
#8498=CARTESIAN_POINT('Origin',(5.11429163215176E-16,0.,86.8));
#8499=CARTESIAN_POINT('',(-6.00000000000001,-1.,86.8));
#8500=CARTESIAN_POINT('',(-6.00000000000001,0.,86.8));
#8501=CARTESIAN_POINT('Origin',(5.11429163215176E-16,-1.,86.8));
#8502=CARTESIAN_POINT('Origin',(5.11429163215176E-16,0.,86.8));
#8503=CARTESIAN_POINT('',(-7.00000000000001,-1.,86.8));
#8504=CARTESIAN_POINT('Origin',(5.11429163215176E-16,-1.,86.8));
#8505=CARTESIAN_POINT('',(-7.00000000000001,0.,86.8));
#8506=CARTESIAN_POINT('Origin',(0.,-1.,86.8));
#8507=CARTESIAN_POINT('Origin',(0.,0.,50.));
#8508=CARTESIAN_POINT('Origin',(-35.,0.,100.));
#8509=CARTESIAN_POINT('',(35.,2.,100.));
#8510=CARTESIAN_POINT('',(35.,0.,100.));
#8511=CARTESIAN_POINT('',(-35.,2.,100.));
#8512=CARTESIAN_POINT('',(-35.,2.,100.));
#8513=CARTESIAN_POINT('',(-35.,0.,100.));
#8514=CARTESIAN_POINT('Origin',(-35.,0.,0.));
#8515=CARTESIAN_POINT('',(-35.,2.,0.));
#8516=CARTESIAN_POINT('',(-35.,2.,0.));
#8517=CARTESIAN_POINT('',(-35.,0.,0.));
#8518=CARTESIAN_POINT('Origin',(35.,0.,0.));
#8519=CARTESIAN_POINT('',(35.,2.,0.));
#8520=CARTESIAN_POINT('',(35.,2.,0.));
#8521=CARTESIAN_POINT('',(35.,0.,0.));
#8522=CARTESIAN_POINT('Origin',(35.,0.,100.));
#8523=CARTESIAN_POINT('',(35.,2.,100.));
#8524=CARTESIAN_POINT('Origin',(0.,2.,50.));
#8525=CARTESIAN_POINT('Origin',(0.,0.,50.));
#8526=CARTESIAN_POINT('',(0.,0.,0.));
#8527=CARTESIAN_POINT('Origin',(3.64981768126446E-16,-4.00000000000001,
86.8));
#8528=CARTESIAN_POINT('',(-1.99999999999999,-4.00000000000001,86.8));
#8529=CARTESIAN_POINT('Origin',(3.64981768126446E-16,-4.00000000000001,
86.8));
#8530=CARTESIAN_POINT('',(-1.99999999999999,-6.00000000000001,86.8));
#8531=CARTESIAN_POINT('',(-1.99999999999999,-4.00000000000001,86.8));
#8532=CARTESIAN_POINT('Origin',(8.74260119701567E-17,-6.00000000000001,
86.8));
#8533=CARTESIAN_POINT('Origin',(3.64981768126446E-16,-4.00000000000001,
86.8));
#8534=CARTESIAN_POINT('',(-2.99999999999999,-6.00000000000001,86.8));
#8535=CARTESIAN_POINT('Origin',(8.74260119701567E-17,-6.00000000000001,
86.8));
#8536=CARTESIAN_POINT('',(-2.99999999999999,-4.00000000000001,86.8));
#8537=CARTESIAN_POINT('',(-2.99999999999999,-4.00000000000001,86.8));
#8538=CARTESIAN_POINT('Origin',(3.64981768126446E-16,-4.00000000000001,
86.8));
#8539=CARTESIAN_POINT('Origin',(-5.55111416207579E-17,-6.00000000000001,
86.8));
#8540=CARTESIAN_POINT('Origin',(2.22044614535531E-16,-4.00000000000001,
86.8));
#8541=CARTESIAN_POINT('',(0.,0.,0.));
#8542=CARTESIAN_POINT('Origin',(3.65,-7.00000000000001,86.8));
#8543=CARTESIAN_POINT('',(4.,-7.00000000000001,87.22));
#8544=CARTESIAN_POINT('Origin',(4.,-7.00000000000001,86.8));
#8545=CARTESIAN_POINT('',(3.65,-7.00000000000001,87.57));
#8546=CARTESIAN_POINT('Origin',(3.65,-7.00000000000001,87.22));
#8547=CARTESIAN_POINT('',(3.65,-7.77000000000001,86.8));
#8548=CARTESIAN_POINT('Origin',(3.65,-7.00000000000001,86.8));
#8549=CARTESIAN_POINT('Origin',(3.65,-7.00000000000001,86.8));
#8550=CARTESIAN_POINT('Origin',(0.,-7.00000000000001,86.8));
#8551=CARTESIAN_POINT('',(1.99999999999999,-7.77000000000002,86.8));
#8552=CARTESIAN_POINT('',(0.,-7.77000000000002,86.8));
#8553=CARTESIAN_POINT('',(1.84583314522196,-7.00000000000001,87.57));
#8554=CARTESIAN_POINT('Ctrl Pts',(1.84583314522195,-7.00000000000001,87.57));
#8555=CARTESIAN_POINT('Ctrl Pts',(1.84583314522195,-6.90217004673391,87.57));
#8556=CARTESIAN_POINT('Ctrl Pts',(1.854432195632,-6.79861108012537,87.5502407729135));
#8557=CARTESIAN_POINT('Ctrl Pts',(1.88442049625666,-6.60925764081413,87.4713711812985));
#8558=CARTESIAN_POINT('Ctrl Pts',(1.90526976397196,-6.52335991547568,87.412304358503));
#8559=CARTESIAN_POINT('Ctrl Pts',(1.94363570580007,-6.38775381022663,87.2766982532539));
#8560=CARTESIAN_POINT('Ctrl Pts',(1.96378848031407,-6.32864270522496,87.1907782243559));
#8561=CARTESIAN_POINT('Ctrl Pts',(1.99214343577073,-6.24973944011141,87.0013388884702));
#8562=CARTESIAN_POINT('Ctrl Pts',(1.99999999999999,-6.23000000000001,86.8977460602273));
#8563=CARTESIAN_POINT('Ctrl Pts',(1.99999999999999,-6.23000000000001,86.7022539397726));
#8564=CARTESIAN_POINT('Ctrl Pts',(1.99214343577073,-6.24973944011141,86.5986611115298));
#8565=CARTESIAN_POINT('Ctrl Pts',(1.96378848031407,-6.32864270522496,86.4092217756441));
#8566=CARTESIAN_POINT('Ctrl Pts',(1.94363570580007,-6.38775381022663,86.3233017467461));
#8567=CARTESIAN_POINT('Ctrl Pts',(1.90526976397196,-6.52335991547568,86.187695641497));
#8568=CARTESIAN_POINT('Ctrl Pts',(1.88442049625666,-6.60925764081413,86.1286288187015));
#8569=CARTESIAN_POINT('Ctrl Pts',(1.854432195632,-6.79861108012537,86.0497592270865));
#8570=CARTESIAN_POINT('Ctrl Pts',(1.84583314522195,-6.90217004673391,86.03));
#8571=CARTESIAN_POINT('Ctrl Pts',(1.84583314522195,-7.09782995326611,86.03));
#8572=CARTESIAN_POINT('Ctrl Pts',(1.854432195632,-7.20138891987465,86.0497592270865));
#8573=CARTESIAN_POINT('Ctrl Pts',(1.88442049625666,-7.39074235918589,86.1286288187015));
#8574=CARTESIAN_POINT('Ctrl Pts',(1.90526976397196,-7.47664008452434,86.187695641497));
#8575=CARTESIAN_POINT('Ctrl Pts',(1.94363570580007,-7.61224618977339,86.3233017467461));
#8576=CARTESIAN_POINT('Ctrl Pts',(1.96378848031406,-7.67135729477505,86.4092217756441));
#8577=CARTESIAN_POINT('Ctrl Pts',(1.99214343577073,-7.75026055988861,86.5986611115297));
#8578=CARTESIAN_POINT('Ctrl Pts',(1.99999999999999,-7.77000000000002,86.7022539397726));
#8579=CARTESIAN_POINT('Ctrl Pts',(1.99999999999999,-7.77000000000002,86.8));
#8580=CARTESIAN_POINT('Ctrl Pts',(1.99999999999999,-7.77000000000002,86.8));
#8581=CARTESIAN_POINT('Ctrl Pts',(1.99999999999999,-7.77000000000002,86.8977460602273));
#8582=CARTESIAN_POINT('Ctrl Pts',(1.99214343577073,-7.75026055988861,87.0013388884702));
#8583=CARTESIAN_POINT('Ctrl Pts',(1.96378848031407,-7.67135729477507,87.1907782243559));
#8584=CARTESIAN_POINT('Ctrl Pts',(1.94363570580007,-7.61224618977339,87.2766982532539));
#8585=CARTESIAN_POINT('Ctrl Pts',(1.90526976397196,-7.47664008452434,87.412304358503));
#8586=CARTESIAN_POINT('Ctrl Pts',(1.88442049625666,-7.39074235918589,87.4713711812985));
#8587=CARTESIAN_POINT('Ctrl Pts',(1.854432195632,-7.20138891987465,87.5502407729135));
#8588=CARTESIAN_POINT('Ctrl Pts',(1.84583314522195,-7.09782995326611,87.57));
#8589=CARTESIAN_POINT('Ctrl Pts',(1.84583314522195,-7.00000000000001,87.57));
#8590=CARTESIAN_POINT('Origin',(4.,-7.00000000000001,86.8));
#8591=CARTESIAN_POINT('Origin',(-3.65,-7.00000000000001,86.8));
#8592=CARTESIAN_POINT('',(-4.,-7.00000000000001,86.38));
#8593=CARTESIAN_POINT('Origin',(-4.,-7.00000000000001,86.8));
#8594=CARTESIAN_POINT('',(-3.65,-7.00000000000001,86.03));
#8595=CARTESIAN_POINT('Origin',(-3.65,-7.00000000000001,86.38));
#8596=CARTESIAN_POINT('',(-3.65,-7.77000000000001,86.8));
#8597=CARTESIAN_POINT('Origin',(-3.65,-7.00000000000001,86.8));
#8598=CARTESIAN_POINT('Origin',(-3.65,-7.00000000000001,86.8));
#8599=CARTESIAN_POINT('Origin',(0.,-7.00000000000001,86.8));
#8600=CARTESIAN_POINT('',(-1.84583314522196,-7.00000000000001,87.57));
#8601=CARTESIAN_POINT('',(-1.99999999999999,-7.77000000000002,86.8));
#8602=CARTESIAN_POINT('Ctrl Pts',(-1.84583314522195,-7.00000000000001,87.57));
#8603=CARTESIAN_POINT('Ctrl Pts',(-1.84583314522195,-7.09782995326611,87.57));
#8604=CARTESIAN_POINT('Ctrl Pts',(-1.854432195632,-7.20138891987465,87.5502407729135));
#8605=CARTESIAN_POINT('Ctrl Pts',(-1.88442049625666,-7.39074235918589,87.4713711812985));
#8606=CARTESIAN_POINT('Ctrl Pts',(-1.90526976397196,-7.47664008452434,87.412304358503));
#8607=CARTESIAN_POINT('Ctrl Pts',(-1.94363570580007,-7.61224618977339,87.2766982532539));
#8608=CARTESIAN_POINT('Ctrl Pts',(-1.96378848031407,-7.67135729477507,87.1907782243559));
#8609=CARTESIAN_POINT('Ctrl Pts',(-1.99214343577073,-7.75026055988861,87.0013388884702));
#8610=CARTESIAN_POINT('Ctrl Pts',(-1.99999999999999,-7.77000000000002,86.8977460602273));
#8611=CARTESIAN_POINT('Ctrl Pts',(-1.99999999999999,-7.77000000000002,86.8));
#8612=CARTESIAN_POINT('',(-1.99999999999999,-6.23,86.8));
#8613=CARTESIAN_POINT('Ctrl Pts',(-1.99999999999999,-6.23000000000001,86.8));
#8614=CARTESIAN_POINT('Ctrl Pts',(-1.99999999999999,-6.23000000000001,86.8977460602273));
#8615=CARTESIAN_POINT('Ctrl Pts',(-1.99214343577073,-6.24973944011141,87.0013388884702));
#8616=CARTESIAN_POINT('Ctrl Pts',(-1.96378848031407,-6.32864270522496,87.1907782243559));
#8617=CARTESIAN_POINT('Ctrl Pts',(-1.94363570580007,-6.38775381022663,87.2766982532539));
#8618=CARTESIAN_POINT('Ctrl Pts',(-1.90526976397196,-6.52335991547568,87.412304358503));
#8619=CARTESIAN_POINT('Ctrl Pts',(-1.88442049625666,-6.60925764081413,87.4713711812985));
#8620=CARTESIAN_POINT('Ctrl Pts',(-1.854432195632,-6.79861108012537,87.5502407729135));
#8621=CARTESIAN_POINT('Ctrl Pts',(-1.84583314522195,-6.90217004673391,87.57));
#8622=CARTESIAN_POINT('Ctrl Pts',(-1.84583314522195,-7.00000000000001,87.57));
#8623=CARTESIAN_POINT('Ctrl Pts',(-1.99999999999999,-7.77000000000002,86.8));
#8624=CARTESIAN_POINT('Ctrl Pts',(-1.99999999999999,-7.77000000000002,86.7022539397726));
#8625=CARTESIAN_POINT('Ctrl Pts',(-1.99214343577073,-7.75026055988861,86.5986611115298));
#8626=CARTESIAN_POINT('Ctrl Pts',(-1.96378848031407,-7.67135729477507,86.4092217756441));
#8627=CARTESIAN_POINT('Ctrl Pts',(-1.94363570580007,-7.61224618977339,86.3233017467461));
#8628=CARTESIAN_POINT('Ctrl Pts',(-1.90526976397196,-7.47664008452434,86.187695641497));
#8629=CARTESIAN_POINT('Ctrl Pts',(-1.88442049625666,-7.39074235918589,86.1286288187015));
#8630=CARTESIAN_POINT('Ctrl Pts',(-1.854432195632,-7.20138891987465,86.0497592270865));
#8631=CARTESIAN_POINT('Ctrl Pts',(-1.84583314522195,-7.09782995326611,86.03));
#8632=CARTESIAN_POINT('Ctrl Pts',(-1.84583314522195,-6.90217004673391,86.03));
#8633=CARTESIAN_POINT('Ctrl Pts',(-1.854432195632,-6.79861108012537,86.0497592270865));
#8634=CARTESIAN_POINT('Ctrl Pts',(-1.88442049625666,-6.60925764081413,86.1286288187015));
#8635=CARTESIAN_POINT('Ctrl Pts',(-1.90526976397196,-6.52335991547568,86.187695641497));
#8636=CARTESIAN_POINT('Ctrl Pts',(-1.94363570580007,-6.38775381022663,86.3233017467461));
#8637=CARTESIAN_POINT('Ctrl Pts',(-1.96378848031407,-6.32864270522496,86.4092217756441));
#8638=CARTESIAN_POINT('Ctrl Pts',(-1.99214343577073,-6.24973944011141,86.5986611115298));
#8639=CARTESIAN_POINT('Ctrl Pts',(-1.99999999999999,-6.23000000000001,86.7022539397726));
#8640=CARTESIAN_POINT('Ctrl Pts',(-1.99999999999999,-6.23000000000001,86.8));
#8641=CARTESIAN_POINT('',(0.,-7.77000000000002,86.8));
#8642=CARTESIAN_POINT('Origin',(-4.,-7.00000000000001,86.8));
#8643=CARTESIAN_POINT('Origin',(1.0547118830044E-15,1.99999999999999,86.8));
#8644=CARTESIAN_POINT('',(-1.99999999999999,1.99999999999999,86.8));
#8645=CARTESIAN_POINT('Origin',(9.20093280439024E-16,1.99999999999999,86.8));
#8646=CARTESIAN_POINT('Origin',(3.64981768126446E-16,-4.00000000000001,
86.8));
#8647=CARTESIAN_POINT('',(-1.99999999999999,-8.00000000000001,86.8));
#8648=CARTESIAN_POINT('Origin',(8.74260119701567E-17,-8.00000000000001,
86.8));
#8649=CARTESIAN_POINT('',(-1.99999999999999,-4.00000000000001,86.8));
#8650=CARTESIAN_POINT('',(-1.99999999999999,-4.00000000000001,86.8));
#8651=CARTESIAN_POINT('Origin',(2.22044614535531E-16,-8.00000000000001,
86.8));
#8652=CARTESIAN_POINT('',(0.,0.,0.));
#8653=CARTESIAN_POINT('Origin',(19.5922696666578,-2.,67.8541394183561));
#8654=CARTESIAN_POINT('',(19.3381754681079,-2.,68.1935760714115));
#8655=CARTESIAN_POINT('',(19.5922696666578,-2.,67.8541394183561));
#8656=CARTESIAN_POINT('',(19.3381754681079,-2.,68.1935760714115));
#8657=CARTESIAN_POINT('',(19.3381754681079,-4.,68.1935760714115));
#8658=CARTESIAN_POINT('',(19.3381754681079,-2.,68.1935760714115));
#8659=CARTESIAN_POINT('',(19.5922696666578,-4.,67.8541394183561));
#8660=CARTESIAN_POINT('',(19.3381754681079,-4.,68.1935760714115));
#8661=CARTESIAN_POINT('',(19.5922696666578,-2.,67.8541394183561));
#8662=CARTESIAN_POINT('Origin',(14.3152323211595,-2.,63.1027041772194));
#8663=CARTESIAN_POINT('',(14.3152323211595,-2.,63.1027041772194));
#8664=CARTESIAN_POINT('',(19.5922696666578,-2.,67.8541394183561));
#8665=CARTESIAN_POINT('',(14.3152323211595,-4.,63.1027041772194));
#8666=CARTESIAN_POINT('',(19.5922696666578,-4.,67.8541394183561));
#8667=CARTESIAN_POINT('',(14.3152323211594,-2.,63.1027041772194));
#8668=CARTESIAN_POINT('Origin',(19.3381754681079,-2.,68.1935760714115));
#8669=CARTESIAN_POINT('',(12.3948017935724,-2.,64.2849475767401));
#8670=CARTESIAN_POINT('',(19.3381754681079,-2.,68.1935760714115));
#8671=CARTESIAN_POINT('',(12.3948017935724,-4.,64.2849475767401));
#8672=CARTESIAN_POINT('',(12.3948017935724,-2.,64.2849475767401));
#8673=CARTESIAN_POINT('',(19.3381754681079,-4.,68.1935760714115));
#8674=CARTESIAN_POINT('Origin',(5.11429163215176E-16,-2.,42.));
#8675=CARTESIAN_POINT('',(16.7572467664191,-4.,61.2209438064143));
#8676=CARTESIAN_POINT('Origin',(5.11429163215176E-16,-4.,42.));
#8677=CARTESIAN_POINT('',(16.7572467664191,-2.,61.2209438064143));
#8678=CARTESIAN_POINT('',(16.7572467664191,-2.,61.2209438064143));
#8679=CARTESIAN_POINT('Origin',(5.11429163215176E-16,-2.,42.));
#8680=CARTESIAN_POINT('Origin',(5.11429163215176E-16,-2.,42.));
#8681=CARTESIAN_POINT('',(9.61491124257648,-2.,65.6178636162837));
#8682=CARTESIAN_POINT('Origin',(5.11429163215176E-16,-2.,42.));
#8683=CARTESIAN_POINT('',(9.61491124257648,-4.,65.6178636162837));
#8684=CARTESIAN_POINT('',(9.61491124257649,-2.,65.6178636162837));
#8685=CARTESIAN_POINT('Origin',(5.11429163215176E-16,-4.,42.));
#8686=CARTESIAN_POINT('Origin',(24.5395094084795,-2.,63.21570252775));
#8687=CARTESIAN_POINT('',(24.3615406262698,-2.,63.6005508299847));
#8688=CARTESIAN_POINT('',(24.5395094084795,-2.,63.21570252775));
#8689=CARTESIAN_POINT('',(24.3615406262698,-2.,63.6005508299847));
#8690=CARTESIAN_POINT('',(24.3615406262698,-4.,63.6005508299847));
#8691=CARTESIAN_POINT('',(24.3615406262698,-2.,63.6005508299847));
#8692=CARTESIAN_POINT('',(24.5395094084795,-4.,63.21570252775));
#8693=CARTESIAN_POINT('',(24.3615406262698,-4.,63.6005508299847));
#8694=CARTESIAN_POINT('',(24.5395094084795,-2.,63.21570252775));
#8695=CARTESIAN_POINT('Origin',(18.3899090552018,-2.,59.6652553036011));
#8696=CARTESIAN_POINT('',(18.3899090552018,-2.,59.6652553036011));
#8697=CARTESIAN_POINT('',(24.5395094084795,-2.,63.21570252775));
#8698=CARTESIAN_POINT('',(18.3899090552018,-4.,59.6652553036011));
#8699=CARTESIAN_POINT('',(24.5395094084795,-4.,63.21570252775));
#8700=CARTESIAN_POINT('',(18.3899090552018,-2.,59.6652553036011));
#8701=CARTESIAN_POINT('Origin',(24.3615406262698,-2.,63.6005508299847));
#8702=CARTESIAN_POINT('',(24.3615406262698,-2.,63.6005508299847));
#8703=CARTESIAN_POINT('',(24.3615406262698,-4.,63.6005508299847));
#8704=CARTESIAN_POINT('Origin',(5.11429163215176E-16,-2.,42.));
#8705=CARTESIAN_POINT('',(20.3873196453819,-4.,57.3168925594268));
#8706=CARTESIAN_POINT('Origin',(5.11429163215176E-16,-4.,42.));
#8707=CARTESIAN_POINT('',(20.3873196453819,-2.,57.3168925594268));
#8708=CARTESIAN_POINT('',(20.3873196453819,-2.,57.3168925594268));
#8709=CARTESIAN_POINT('Origin',(5.11429163215176E-16,-2.,42.));
#8710=CARTESIAN_POINT('Origin',(28.41425483552,-2.,57.6500376324455));
#8711=CARTESIAN_POINT('',(28.3201895594221,-2.,58.0634778663449));
#8712=CARTESIAN_POINT('',(28.41425483552,-2.,57.6500376324455));
#8713=CARTESIAN_POINT('',(28.3201895594221,-2.,58.0634778663449));
#8714=CARTESIAN_POINT('',(28.3201895594221,-4.,58.0634778663449));
#8715=CARTESIAN_POINT('',(28.3201895594221,-2.,58.0634778663449));
#8716=CARTESIAN_POINT('',(28.41425483552,-4.,57.6500376324455));
#8717=CARTESIAN_POINT('',(28.3201895594221,-4.,58.0634778663449));
#8718=CARTESIAN_POINT('',(28.41425483552,-2.,57.6500376324455));
#8719=CARTESIAN_POINT('Origin',(21.6608585189577,-2.,55.4557500059157));
#8720=CARTESIAN_POINT('',(21.6608585189577,-2.,55.4557500059157));
#8721=CARTESIAN_POINT('',(28.41425483552,-2.,57.6500376324455));
#8722=CARTESIAN_POINT('',(21.6608585189577,-4.,55.4557500059157));
#8723=CARTESIAN_POINT('',(28.41425483552,-4.,57.6500376324455));
#8724=CARTESIAN_POINT('',(21.6608585189577,-2.,55.4557500059157));
#8725=CARTESIAN_POINT('Origin',(28.3201895594221,-2.,58.0634778663449));
#8726=CARTESIAN_POINT('',(28.3201895594221,-2.,58.0634778663449));
#8727=CARTESIAN_POINT('',(28.3201895594221,-4.,58.0634778663449));
#8728=CARTESIAN_POINT('Origin',(5.11429163215176E-16,-2.,42.));
#8729=CARTESIAN_POINT('',(23.1263688266279,-4.,52.7434196089874));
#8730=CARTESIAN_POINT('Origin',(5.11429163215176E-16,-4.,42.));
#8731=CARTESIAN_POINT('',(23.1263688266279,-2.,52.7434196089874));
#8732=CARTESIAN_POINT('',(23.1263688266279,-2.,52.7434196089874));
#8733=CARTESIAN_POINT('Origin',(5.11429163215176E-16,-2.,42.));
#8734=CARTESIAN_POINT('Origin',(31.0471609795261,-2.,51.4003909953907));
#8735=CARTESIAN_POINT('',(31.0411103134807,-2.,51.8243538388269));
#8736=CARTESIAN_POINT('',(31.0471609795261,-2.,51.4003909953907));
#8737=CARTESIAN_POINT('',(31.0411103134807,-2.,51.8243538388269));
#8738=CARTESIAN_POINT('',(31.0411103134807,-4.,51.8243538388269));
#8739=CARTESIAN_POINT('',(31.0411103134807,-2.,51.8243538388269));
#8740=CARTESIAN_POINT('',(31.0471609795261,-4.,51.4003909953907));
#8741=CARTESIAN_POINT('',(31.0411103134807,-4.,51.8243538388269));
#8742=CARTESIAN_POINT('',(31.0471609795261,-2.,51.4003909953907));
#8743=CARTESIAN_POINT('Origin',(23.9851245251038,-2.,50.6581638651196));
#8744=CARTESIAN_POINT('',(23.9851245251038,-2.,50.6581638651196));
#8745=CARTESIAN_POINT('',(31.0471609795261,-2.,51.4003909953907));
#8746=CARTESIAN_POINT('',(23.9851245251038,-4.,50.6581638651196));
#8747=CARTESIAN_POINT('',(31.0471609795261,-4.,51.4003909953907));
#8748=CARTESIAN_POINT('',(23.9851245251038,-2.,50.6581638651196));
#8749=CARTESIAN_POINT('Origin',(31.0411103134807,-2.,51.8243538388269));
#8750=CARTESIAN_POINT('',(31.0411103134807,-2.,51.8243538388269));
#8751=CARTESIAN_POINT('',(31.0411103134807,-4.,51.8243538388269));
#8752=CARTESIAN_POINT('Origin',(5.11429163215176E-16,-2.,42.));
#8753=CARTESIAN_POINT('',(24.8546847175204,-4.,47.7004076689882));
#8754=CARTESIAN_POINT('Origin',(5.11429163215176E-16,-4.,42.));
#8755=CARTESIAN_POINT('',(24.8546847175204,-2.,47.7004076689882));
#8756=CARTESIAN_POINT('',(24.8546847175204,-2.,47.7004076689882));
#8757=CARTESIAN_POINT('Origin',(5.11429163215176E-16,-2.,42.));
#8758=CARTESIAN_POINT('Origin',(32.3231572079194,-2.,44.7399021637567));
#8759=CARTESIAN_POINT('',(32.405385595067,-2.,45.1558584060722));
#8760=CARTESIAN_POINT('',(32.3231572079194,-2.,44.7399021637567));
#8761=CARTESIAN_POINT('',(32.405385595067,-2.,45.1558584060722));
#8762=CARTESIAN_POINT('',(32.405385595067,-4.,45.1558584060722));
#8763=CARTESIAN_POINT('',(32.405385595067,-2.,45.1558584060722));
#8764=CARTESIAN_POINT('',(32.3231572079194,-4.,44.7399021637567));
#8765=CARTESIAN_POINT('',(32.405385595067,-4.,45.1558584060722));
#8766=CARTESIAN_POINT('',(32.3231572079194,-2.,44.7399021637567));
#8767=CARTESIAN_POINT('Origin',(25.2611254961061,-2.,45.482174416938));
#8768=CARTESIAN_POINT('',(25.2611254961061,-2.,45.482174416938));
#8769=CARTESIAN_POINT('',(32.3231572079194,-2.,44.7399021637567));
#8770=CARTESIAN_POINT('',(25.2611254961061,-4.,45.482174416938));
#8771=CARTESIAN_POINT('',(32.3231572079194,-4.,44.7399021637567));
#8772=CARTESIAN_POINT('',(25.2611254961061,-2.,45.482174416938));
#8773=CARTESIAN_POINT('Origin',(32.405385595067,-2.,45.1558584060722));
#8774=CARTESIAN_POINT('',(32.405385595067,-2.,45.1558584060722));
#8775=CARTESIAN_POINT('',(32.405385595067,-4.,45.1558584060722));
#8776=CARTESIAN_POINT('Origin',(5.11429163215176E-16,-2.,42.));
#8777=CARTESIAN_POINT('',(25.4967316202476,-4.,42.4082605602634));
#8778=CARTESIAN_POINT('Origin',(5.11429163215176E-16,-4.,42.));
#8779=CARTESIAN_POINT('',(25.4967316202476,-2.,42.4082605602634));
#8780=CARTESIAN_POINT('',(25.4967316202476,-2.,42.4082605602634));
#8781=CARTESIAN_POINT('Origin',(5.11429163215176E-16,-2.,42.));
#8782=CARTESIAN_POINT('Origin',(30.643092052405,-2.,31.3560127197245));
#8783=CARTESIAN_POINT('',(30.8873960676387,-2.,31.702562357316));
#8784=CARTESIAN_POINT('',(30.643092052405,-2.,31.3560127197245));
#8785=CARTESIAN_POINT('',(30.8873960676387,-2.,31.702562357316));
#8786=CARTESIAN_POINT('',(30.8873960676387,-4.,31.702562357316));
#8787=CARTESIAN_POINT('',(30.8873960676387,-2.,31.702562357316));
#8788=CARTESIAN_POINT('',(30.643092052405,-4.,31.3560127197245));
#8789=CARTESIAN_POINT('',(30.8873960676387,-4.,31.702562357316));
#8790=CARTESIAN_POINT('',(30.643092052405,-2.,31.3560127197245));
#8791=CARTESIAN_POINT('Origin',(24.4935143848573,-2.,34.9064992367103));
#8792=CARTESIAN_POINT('',(24.4935143848573,-2.,34.9064992367103));
#8793=CARTESIAN_POINT('',(30.643092052405,-2.,31.3560127197245));
#8794=CARTESIAN_POINT('',(24.4935143848573,-4.,34.9064992367103));
#8795=CARTESIAN_POINT('',(30.643092052405,-4.,31.3560127197245));
#8796=CARTESIAN_POINT('',(24.4935143848573,-2.,34.9064992367103));
#8797=CARTESIAN_POINT('Origin',(30.8873960676387,-2.,31.702562357316));
#8798=CARTESIAN_POINT('',(25.0244490042775,-2.,37.0982705060036));
#8799=CARTESIAN_POINT('',(30.8873960676387,-2.,31.702562357316));
#8800=CARTESIAN_POINT('',(25.0244490042775,-4.,37.0982705060036));
#8801=CARTESIAN_POINT('',(25.0244490042775,-2.,37.0982705060036));
#8802=CARTESIAN_POINT('',(30.8873960676387,-4.,31.702562357316));
#8803=CARTESIAN_POINT('Origin',(5.11429163215176E-16,-2.,42.));
#8804=CARTESIAN_POINT('',(23.4584778861915,-4.,32.0025095517392));
#8805=CARTESIAN_POINT('Origin',(5.11429163215176E-16,-4.,42.));
#8806=CARTESIAN_POINT('',(23.4584778861915,-2.,32.0025095517392));
#8807=CARTESIAN_POINT('',(23.4584778861915,-2.,32.0025095517392));
#8808=CARTESIAN_POINT('Origin',(5.11429163215176E-16,-2.,42.));
#8809=CARTESIAN_POINT('Origin',(5.11429163215176E-16,-2.,42.));
#8810=CARTESIAN_POINT('',(25.4330940665997,-2.,40.1539972374095));
#8811=CARTESIAN_POINT('Origin',(5.11429163215176E-16,-2.,42.));
#8812=CARTESIAN_POINT('',(25.4330940665997,-4.,40.1539972374095));
#8813=CARTESIAN_POINT('',(25.4330940665997,-2.,40.1539972374095));
#8814=CARTESIAN_POINT('Origin',(5.11429163215176E-16,-4.,42.));
#8815=CARTESIAN_POINT('Origin',(32.1864763626099,-2.,37.9596664600572));
#8816=CARTESIAN_POINT('',(32.3533900278565,-2.,38.3494368174833));
#8817=CARTESIAN_POINT('',(32.1864763626099,-2.,37.9596664600572));
#8818=CARTESIAN_POINT('',(32.3533900278565,-2.,38.3494368174833));
#8819=CARTESIAN_POINT('',(32.3533900278565,-4.,38.3494368174833));
#8820=CARTESIAN_POINT('',(32.3533900278565,-2.,38.3494368174833));
#8821=CARTESIAN_POINT('',(32.1864763626099,-4.,37.9596664600572));
#8822=CARTESIAN_POINT('',(32.3533900278565,-4.,38.3494368174833));
#8823=CARTESIAN_POINT('',(32.1864763626099,-2.,37.9596664600572));
#8824=CARTESIAN_POINT('Origin',(25.4330940665997,-2.,40.1539972374095));
#8825=CARTESIAN_POINT('',(32.1864763626099,-2.,37.9596664600572));
#8826=CARTESIAN_POINT('',(32.1864763626099,-4.,37.9596664600572));
#8827=CARTESIAN_POINT('Origin',(32.3533900278565,-2.,38.3494368174833));
#8828=CARTESIAN_POINT('',(32.3533900278565,-2.,38.3494368174833));
#8829=CARTESIAN_POINT('',(32.3533900278565,-4.,38.3494368174833));
#8830=CARTESIAN_POINT('Origin',(27.7604575776403,-2.,25.2175522990576));
#8831=CARTESIAN_POINT('',(28.0714746850947,-2.,25.5057353347221));
#8832=CARTESIAN_POINT('',(27.7604575776403,-2.,25.2175522990576));
#8833=CARTESIAN_POINT('',(28.0714746850947,-2.,25.5057353347221));
#8834=CARTESIAN_POINT('',(28.0714746850947,-4.,25.5057353347221));
#8835=CARTESIAN_POINT('',(28.0714746850947,-2.,25.5057353347221));
#8836=CARTESIAN_POINT('',(27.7604575776403,-4.,25.2175522990576));
#8837=CARTESIAN_POINT('',(28.0714746850947,-4.,25.5057353347221));
#8838=CARTESIAN_POINT('',(27.7604575776403,-2.,25.2175522990576));
#8839=CARTESIAN_POINT('Origin',(22.4834505915744,-2.,29.96902125776));
#8840=CARTESIAN_POINT('',(22.4834505915744,-2.,29.96902125776));
#8841=CARTESIAN_POINT('',(27.7604575776403,-2.,25.2175522990576));
#8842=CARTESIAN_POINT('',(22.4834505915744,-4.,29.96902125776));
#8843=CARTESIAN_POINT('',(27.7604575776403,-4.,25.2175522990576));
#8844=CARTESIAN_POINT('',(22.4834505915744,-2.,29.96902125776));
#8845=CARTESIAN_POINT('Origin',(28.0714746850947,-2.,25.5057353347221));
#8846=CARTESIAN_POINT('',(28.0714746850947,-2.,25.5057353347221));
#8847=CARTESIAN_POINT('',(28.0714746850947,-4.,25.5057353347221));
#8848=CARTESIAN_POINT('Origin',(5.11429163215176E-16,-2.,42.));
#8849=CARTESIAN_POINT('',(20.8672587182129,-4.,27.3436869033454));
#8850=CARTESIAN_POINT('Origin',(5.11429163215176E-16,-4.,42.));
#8851=CARTESIAN_POINT('',(20.8672587182129,-2.,27.3436869033454));
#8852=CARTESIAN_POINT('',(20.8672587182129,-2.,27.3436869033454));
#8853=CARTESIAN_POINT('Origin',(5.11429163215176E-16,-2.,42.));
#8854=CARTESIAN_POINT('Origin',(18.5344034816569,-2.,15.377275809302));
#8855=CARTESIAN_POINT('',(18.9357463479386,-2.,15.5140420582778));
#8856=CARTESIAN_POINT('',(18.5344034816569,-2.,15.377275809302));
#8857=CARTESIAN_POINT('',(18.9357463479386,-2.,15.5140420582778));
#8858=CARTESIAN_POINT('',(18.9357463479386,-4.,15.5140420582778));
#8859=CARTESIAN_POINT('',(18.9357463479386,-2.,15.5140420582778));
#8860=CARTESIAN_POINT('',(18.5344034816569,-4.,15.377275809302));
#8861=CARTESIAN_POINT('',(18.9357463479386,-4.,15.5140420582778));
#8862=CARTESIAN_POINT('',(18.5344034816569,-2.,15.377275809302));
#8863=CARTESIAN_POINT('Origin',(15.6462142535297,-2.,21.8643108006543));
#8864=CARTESIAN_POINT('',(15.6462142535297,-2.,21.8643108006543));
#8865=CARTESIAN_POINT('',(18.5344034816569,-2.,15.377275809302));
#8866=CARTESIAN_POINT('',(15.6462142535297,-4.,21.8643108006543));
#8867=CARTESIAN_POINT('',(18.5344034816569,-4.,15.377275809302));
#8868=CARTESIAN_POINT('',(15.6462142535297,-2.,21.8643108006543));
#8869=CARTESIAN_POINT('Origin',(18.9357463479386,-2.,15.5140420582778));
#8870=CARTESIAN_POINT('',(17.3640402120316,-2.,23.3254154660686));
#8871=CARTESIAN_POINT('',(18.9357463479386,-2.,15.5140420582778));
#8872=CARTESIAN_POINT('',(17.3640402120316,-4.,23.3254154660686));
#8873=CARTESIAN_POINT('',(17.3640402120316,-2.,23.3254154660686));
#8874=CARTESIAN_POINT('',(18.9357463479386,-4.,15.5140420582778));
#8875=CARTESIAN_POINT('Origin',(5.11429163215176E-16,-2.,42.));
#8876=CARTESIAN_POINT('',(13.1019298266752,-4.,20.1233129835233));
#8877=CARTESIAN_POINT('Origin',(5.11429163215176E-16,-4.,42.));
#8878=CARTESIAN_POINT('',(13.1019298266752,-2.,20.1233129835233));
#8879=CARTESIAN_POINT('',(13.1019298266752,-2.,20.1233129835233));
#8880=CARTESIAN_POINT('Origin',(5.11429163215176E-16,-2.,42.));
#8881=CARTESIAN_POINT('Origin',(5.11429163215176E-16,-2.,42.));
#8882=CARTESIAN_POINT('',(19.490752119874,-2.,25.5573547808867));
#8883=CARTESIAN_POINT('Origin',(5.11429163215176E-16,-2.,42.));
#8884=CARTESIAN_POINT('',(19.490752119874,-4.,25.5573547808867));
#8885=CARTESIAN_POINT('',(19.490752119874,-2.,25.5573547808867));
#8886=CARTESIAN_POINT('Origin',(5.11429163215176E-16,-4.,42.));
#8887=CARTESIAN_POINT('Origin',(6.1035826439255,-2.,10.1403101919745));
#8888=CARTESIAN_POINT('',(6.52585544136889,-2.,10.1020115273313));
#8889=CARTESIAN_POINT('',(6.1035826439255,-2.,10.1403101919745));
#8890=CARTESIAN_POINT('',(6.52585544136889,-2.,10.1020115273313));
#8891=CARTESIAN_POINT('',(6.52585544136889,-4.,10.1020115273313));
#8892=CARTESIAN_POINT('',(6.52585544136889,-2.,10.1020115273313));
#8893=CARTESIAN_POINT('',(6.1035826439255,-4.,10.1403101919745));
#8894=CARTESIAN_POINT('',(6.52585544136889,-4.,10.1020115273313));
#8895=CARTESIAN_POINT('',(6.1035826439255,-2.,10.1403101919745));
#8896=CARTESIAN_POINT('Origin',(6.10360532965543,-2.,17.2412439331092));
#8897=CARTESIAN_POINT('',(6.10360532965543,-2.,17.2412439331092));
#8898=CARTESIAN_POINT('',(6.1035826439255,-2.,10.1403101919745));
#8899=CARTESIAN_POINT('',(6.10360532965543,-4.,17.2412439331092));
#8900=CARTESIAN_POINT('',(6.1035826439255,-4.,10.1403101919745));
#8901=CARTESIAN_POINT('',(6.10360532965543,-2.,17.2412439331092));
#8902=CARTESIAN_POINT('Origin',(6.52585544136889,-2.,10.1020115273313));
#8903=CARTESIAN_POINT('',(8.26720223785844,-2.,17.8773266995893));
#8904=CARTESIAN_POINT('',(6.52585544136889,-2.,10.1020115273313));
#8905=CARTESIAN_POINT('',(8.26720223785844,-4.,17.8773266995893));
#8906=CARTESIAN_POINT('',(8.26720223785844,-2.,17.8773266995893));
#8907=CARTESIAN_POINT('',(6.52585544136889,-4.,10.1020115273313));
#8908=CARTESIAN_POINT('Origin',(5.11429163215176E-16,-2.,42.));
#8909=CARTESIAN_POINT('',(3.07115824080957,-4.,16.6856169923123));
#8910=CARTESIAN_POINT('Origin',(5.11429163215176E-16,-4.,42.));
#8911=CARTESIAN_POINT('',(3.07115824080957,-2.,16.6856169923123));
#8912=CARTESIAN_POINT('',(3.07115824080957,-2.,16.6856169923123));
#8913=CARTESIAN_POINT('Origin',(5.11429163215176E-16,-2.,42.));
#8914=CARTESIAN_POINT('Origin',(5.11429163215176E-16,-2.,42.));
#8915=CARTESIAN_POINT('',(11.1178617454402,-2.,19.0512930601901));
#8916=CARTESIAN_POINT('Origin',(5.11429163215176E-16,-2.,42.));
#8917=CARTESIAN_POINT('',(11.1178617454402,-4.,19.0512930601901));
#8918=CARTESIAN_POINT('',(11.1178617454402,-2.,19.0512930601901));
#8919=CARTESIAN_POINT('Origin',(5.11429163215176E-16,-4.,42.));
#8920=CARTESIAN_POINT('Origin',(12.5942066959521,-2.,12.1055270417011));
#8921=CARTESIAN_POINT('',(13.0152145597486,-2.,12.1558607460718));
#8922=CARTESIAN_POINT('',(12.5942066959521,-2.,12.1055270417011));
#8923=CARTESIAN_POINT('',(13.0152145597486,-2.,12.1558607460718));
#8924=CARTESIAN_POINT('',(13.0152145597486,-4.,12.1558607460718));
#8925=CARTESIAN_POINT('',(13.0152145597486,-2.,12.1558607460718));
#8926=CARTESIAN_POINT('',(12.5942066959521,-4.,12.1055270417011));
#8927=CARTESIAN_POINT('',(13.0152145597486,-4.,12.1558607460718));
#8928=CARTESIAN_POINT('',(12.5942066959521,-2.,12.1055270417011));
#8929=CARTESIAN_POINT('Origin',(11.1178617454402,-2.,19.0512930601901));
#8930=CARTESIAN_POINT('',(12.5942066959521,-2.,12.1055270417011));
#8931=CARTESIAN_POINT('',(12.5942066959521,-4.,12.1055270417011));
#8932=CARTESIAN_POINT('Origin',(13.0152145597486,-2.,12.1558607460718));
#8933=CARTESIAN_POINT('',(13.0152145597486,-2.,12.1558607460718));
#8934=CARTESIAN_POINT('',(13.0152145597486,-4.,12.1558607460718));
#8935=CARTESIAN_POINT('Origin',(23.6645578972779,-2.,19.8125653740408));
#8936=CARTESIAN_POINT('',(24.0286951569316,-2.,20.0297868262641));
#8937=CARTESIAN_POINT('',(23.6645578972779,-2.,19.8125653740408));
#8938=CARTESIAN_POINT('',(24.0286951569316,-2.,20.0297868262641));
#8939=CARTESIAN_POINT('',(24.0286951569316,-4.,20.0297868262641));
#8940=CARTESIAN_POINT('',(24.0286951569316,-2.,20.0297868262641));
#8941=CARTESIAN_POINT('',(23.6645578972779,-4.,19.8125653740408));
#8942=CARTESIAN_POINT('',(24.0286951569316,-4.,20.0297868262641));
#8943=CARTESIAN_POINT('',(23.6645578972779,-2.,19.8125653740408));
#8944=CARTESIAN_POINT('Origin',(19.490752119874,-2.,25.5573547808867));
#8945=CARTESIAN_POINT('',(23.6645578972779,-2.,19.8125653740408));
#8946=CARTESIAN_POINT('',(23.6645578972779,-4.,19.8125653740408));
#8947=CARTESIAN_POINT('Origin',(24.0286951569316,-2.,20.0297868262641));
#8948=CARTESIAN_POINT('',(24.0286951569316,-2.,20.0297868262641));
#8949=CARTESIAN_POINT('',(24.0286951569316,-4.,20.0297868262641));
#8950=CARTESIAN_POINT('Origin',(-0.653797257879687,-2.,9.5675146666121));
#8951=CARTESIAN_POINT('',(-0.248714874327312,-2.,9.44225746837724));
#8952=CARTESIAN_POINT('',(-0.653797257879687,-2.,9.5675146666121));
#8953=CARTESIAN_POINT('',(-0.248714874327312,-2.,9.44225746837724));
#8954=CARTESIAN_POINT('',(-0.248714874327312,-4.,9.44225746837724));
#8955=CARTESIAN_POINT('',(-0.248714874327312,-2.,9.44225746837724));
#8956=CARTESIAN_POINT('',(-0.653797257879687,-4.,9.5675146666121));
#8957=CARTESIAN_POINT('',(-0.248714874327312,-4.,9.44225746837724));
#8958=CARTESIAN_POINT('',(-0.653797257879687,-2.,9.5675146666121));
#8959=CARTESIAN_POINT('Origin',(0.822592072616804,-2.,16.5132712518442));
#8960=CARTESIAN_POINT('',(0.822592072616804,-2.,16.5132712518442));
#8961=CARTESIAN_POINT('',(-0.653797257879687,-2.,9.5675146666121));
#8962=CARTESIAN_POINT('',(0.822592072616804,-4.,16.5132712518442));
#8963=CARTESIAN_POINT('',(-0.653797257879687,-4.,9.5675146666121));
#8964=CARTESIAN_POINT('',(0.822592072616806,-2.,16.5132712518442));
#8965=CARTESIAN_POINT('Origin',(-0.248714874327312,-2.,9.44225746837724));
#8966=CARTESIAN_POINT('',(-0.248714874327312,-2.,9.44225746837724));
#8967=CARTESIAN_POINT('',(-0.248714874327312,-4.,9.44225746837724));
#8968=CARTESIAN_POINT('Origin',(5.11429163215176E-16,-2.,42.));
#8969=CARTESIAN_POINT('',(-2.25911010841498,-4.,16.600267294358));
#8970=CARTESIAN_POINT('Origin',(5.11429163215176E-16,-4.,42.));
#8971=CARTESIAN_POINT('',(-2.25911010841498,-2.,16.600267294358));
#8972=CARTESIAN_POINT('',(-2.25911010841497,-2.,16.600267294358));
#8973=CARTESIAN_POINT('Origin',(5.11429163215176E-16,-2.,42.));
#8974=CARTESIAN_POINT('Origin',(-7.38260308224823,-2.,10.4121743786501));
#8975=CARTESIAN_POINT('',(-7.01241515654904,-2.,10.2054329874371));
#8976=CARTESIAN_POINT('',(-7.38260308224823,-2.,10.4121743786501));
#8977=CARTESIAN_POINT('',(-7.01241515654904,-2.,10.2054329874371));
#8978=CARTESIAN_POINT('',(-7.01241515654904,-4.,10.2054329874371));
#8979=CARTESIAN_POINT('',(-7.01241515654904,-2.,10.2054329874371));
#8980=CARTESIAN_POINT('',(-7.38260308224823,-4.,10.4121743786501));
#8981=CARTESIAN_POINT('',(-7.01241515654904,-4.,10.2054329874371));
#8982=CARTESIAN_POINT('',(-7.38260308224823,-2.,10.4121743786501));
#8983=CARTESIAN_POINT('Origin',(-4.49437240522989,-2.,16.8991909157671));
#8984=CARTESIAN_POINT('',(-4.49437240522989,-2.,16.8991909157671));
#8985=CARTESIAN_POINT('',(-7.38260308224823,-2.,10.4121743786501));
#8986=CARTESIAN_POINT('',(-4.49437240522989,-4.,16.8991909157671));
#8987=CARTESIAN_POINT('',(-7.38260308224823,-4.,10.4121743786501));
#8988=CARTESIAN_POINT('',(-4.49437240522989,-2.,16.8991909157671));
#8989=CARTESIAN_POINT('Origin',(-7.01241515654904,-2.,10.2054329874371));
#8990=CARTESIAN_POINT('',(-7.01241515654904,-2.,10.2054329874371));
#8991=CARTESIAN_POINT('',(-7.01241515654904,-4.,10.2054329874371));
#8992=CARTESIAN_POINT('Origin',(5.11429163215176E-16,-2.,42.));
#8993=CARTESIAN_POINT('',(-7.49064450548875,-4.,17.6250077970804));
#8994=CARTESIAN_POINT('Origin',(5.11429163215176E-16,-4.,42.));
#8995=CARTESIAN_POINT('',(-7.49064450548875,-2.,17.6250077970804));
#8996=CARTESIAN_POINT('',(-7.49064450548876,-2.,17.6250077970804));
#8997=CARTESIAN_POINT('Origin',(5.11429163215176E-16,-2.,42.));
#8998=CARTESIAN_POINT('Origin',(-28.41425483552,-2.,26.3499623675545));
#8999=CARTESIAN_POINT('',(-28.3201895594221,-2.,25.9365221336551));
#9000=CARTESIAN_POINT('',(-28.41425483552,-2.,26.3499623675545));
#9001=CARTESIAN_POINT('',(-28.3201895594221,-2.,25.9365221336551));
#9002=CARTESIAN_POINT('',(-28.3201895594221,-4.,25.9365221336551));
#9003=CARTESIAN_POINT('',(-28.3201895594221,-2.,25.9365221336551));
#9004=CARTESIAN_POINT('',(-28.41425483552,-4.,26.3499623675545));
#9005=CARTESIAN_POINT('',(-28.3201895594221,-4.,25.9365221336551));
#9006=CARTESIAN_POINT('',(-28.41425483552,-2.,26.3499623675545));
#9007=CARTESIAN_POINT('Origin',(-21.6608585189576,-2.,28.5442499940843));
#9008=CARTESIAN_POINT('',(-21.6608585189576,-2.,28.5442499940843));
#9009=CARTESIAN_POINT('',(-28.41425483552,-2.,26.3499623675545));
#9010=CARTESIAN_POINT('',(-21.6608585189576,-4.,28.5442499940843));
#9011=CARTESIAN_POINT('',(-28.41425483552,-4.,26.3499623675545));
#9012=CARTESIAN_POINT('',(-21.6608585189576,-2.,28.5442499940843));
#9013=CARTESIAN_POINT('Origin',(-28.3201895594221,-2.,25.9365221336551));
#9014=CARTESIAN_POINT('',(-20.3873196453819,-2.,26.6831074405731));
#9015=CARTESIAN_POINT('',(-28.3201895594221,-2.,25.9365221336551));
#9016=CARTESIAN_POINT('',(-20.3873196453819,-4.,26.6831074405731));
#9017=CARTESIAN_POINT('',(-20.3873196453819,-2.,26.6831074405731));
#9018=CARTESIAN_POINT('',(-28.3201895594221,-4.,25.9365221336551));
#9019=CARTESIAN_POINT('Origin',(5.11429163215176E-16,-2.,42.));
#9020=CARTESIAN_POINT('',(-23.1263688266279,-4.,31.2565803910126));
#9021=CARTESIAN_POINT('Origin',(5.11429163215176E-16,-4.,42.));
#9022=CARTESIAN_POINT('',(-23.1263688266279,-2.,31.2565803910126));
#9023=CARTESIAN_POINT('',(-23.1263688266279,-2.,31.2565803910126));
#9024=CARTESIAN_POINT('Origin',(5.11429163215176E-16,-2.,42.));
#9025=CARTESIAN_POINT('Origin',(5.11429163215176E-16,-2.,42.));
#9026=CARTESIAN_POINT('',(-18.3899090552018,-2.,24.3347446963989));
#9027=CARTESIAN_POINT('Origin',(5.11429163215176E-16,-2.,42.));
#9028=CARTESIAN_POINT('',(-18.3899090552018,-4.,24.3347446963989));
#9029=CARTESIAN_POINT('',(-18.3899090552018,-2.,24.3347446963989));
#9030=CARTESIAN_POINT('Origin',(5.11429163215176E-16,-4.,42.));
#9031=CARTESIAN_POINT('Origin',(-13.7887537262625,-2.,12.6373736455454));
#9032=CARTESIAN_POINT('',(-13.4696392471283,-2.,12.3581836522056));
#9033=CARTESIAN_POINT('',(-13.7887537262625,-2.,12.6373736455454));
#9034=CARTESIAN_POINT('',(-13.4696392471283,-2.,12.3581836522056));
#9035=CARTESIAN_POINT('',(-13.4696392471283,-4.,12.3581836522056));
#9036=CARTESIAN_POINT('',(-13.4696392471283,-2.,12.3581836522056));
#9037=CARTESIAN_POINT('',(-13.7887537262625,-4.,12.6373736455454));
#9038=CARTESIAN_POINT('',(-13.4696392471283,-4.,12.3581836522056));
#9039=CARTESIAN_POINT('',(-13.7887537262625,-2.,12.6373736455454));
#9040=CARTESIAN_POINT('Origin',(-9.61491124257647,-2.,18.3821363837163));
#9041=CARTESIAN_POINT('',(-9.61491124257647,-2.,18.3821363837163));
#9042=CARTESIAN_POINT('',(-13.7887537262625,-2.,12.6373736455454));
#9043=CARTESIAN_POINT('',(-9.61491124257647,-4.,18.3821363837163));
#9044=CARTESIAN_POINT('',(-13.7887537262625,-4.,12.6373736455454));
#9045=CARTESIAN_POINT('',(-9.61491124257647,-2.,18.3821363837163));
#9046=CARTESIAN_POINT('Origin',(-13.4696392471283,-2.,12.3581836522056));
#9047=CARTESIAN_POINT('',(-13.4696392471283,-2.,12.3581836522056));
#9048=CARTESIAN_POINT('',(-13.4696392471283,-4.,12.3581836522056));
#9049=CARTESIAN_POINT('Origin',(5.11429163215176E-16,-2.,42.));
#9050=CARTESIAN_POINT('',(-12.3948017935724,-4.,19.7150524232599));
#9051=CARTESIAN_POINT('Origin',(5.11429163215176E-16,-4.,42.));
#9052=CARTESIAN_POINT('',(-12.3948017935724,-2.,19.7150524232599));
#9053=CARTESIAN_POINT('',(-12.3948017935724,-2.,19.7150524232599));
#9054=CARTESIAN_POINT('Origin',(5.11429163215176E-16,-2.,42.));
#9055=CARTESIAN_POINT('Origin',(-19.5922696666578,-2.,16.1458605816439));
#9056=CARTESIAN_POINT('',(-19.3381754681079,-2.,15.8064239285885));
#9057=CARTESIAN_POINT('',(-19.5922696666578,-2.,16.1458605816439));
#9058=CARTESIAN_POINT('',(-19.3381754681079,-2.,15.8064239285885));
#9059=CARTESIAN_POINT('',(-19.3381754681079,-4.,15.8064239285885));
#9060=CARTESIAN_POINT('',(-19.3381754681079,-2.,15.8064239285885));
#9061=CARTESIAN_POINT('',(-19.5922696666578,-4.,16.1458605816439));
#9062=CARTESIAN_POINT('',(-19.3381754681079,-4.,15.8064239285885));
#9063=CARTESIAN_POINT('',(-19.5922696666578,-2.,16.1458605816439));
#9064=CARTESIAN_POINT('Origin',(-14.3152323211595,-2.,20.8972958227806));
#9065=CARTESIAN_POINT('',(-14.3152323211595,-2.,20.8972958227806));
#9066=CARTESIAN_POINT('',(-19.5922696666578,-2.,16.1458605816439));
#9067=CARTESIAN_POINT('',(-14.3152323211595,-4.,20.8972958227806));
#9068=CARTESIAN_POINT('',(-19.5922696666578,-4.,16.1458605816439));
#9069=CARTESIAN_POINT('',(-14.3152323211594,-2.,20.8972958227806));
#9070=CARTESIAN_POINT('Origin',(-19.3381754681079,-2.,15.8064239285885));
#9071=CARTESIAN_POINT('',(-19.3381754681079,-2.,15.8064239285885));
#9072=CARTESIAN_POINT('',(-19.3381754681079,-4.,15.8064239285885));
#9073=CARTESIAN_POINT('Origin',(5.11429163215176E-16,-2.,42.));
#9074=CARTESIAN_POINT('',(-16.7572467664191,-4.,22.7790561935857));
#9075=CARTESIAN_POINT('Origin',(5.11429163215176E-16,-4.,42.));
#9076=CARTESIAN_POINT('',(-16.7572467664191,-2.,22.7790561935857));
#9077=CARTESIAN_POINT('',(-16.7572467664191,-2.,22.7790561935857));
#9078=CARTESIAN_POINT('Origin',(5.11429163215176E-16,-2.,42.));
#9079=CARTESIAN_POINT('Origin',(-24.5395094084795,-2.,20.78429747225));
#9080=CARTESIAN_POINT('',(-24.3615406262698,-2.,20.3994491700153));
#9081=CARTESIAN_POINT('',(-24.5395094084795,-2.,20.78429747225));
#9082=CARTESIAN_POINT('',(-24.3615406262698,-2.,20.3994491700153));
#9083=CARTESIAN_POINT('',(-24.3615406262698,-4.,20.3994491700153));
#9084=CARTESIAN_POINT('',(-24.3615406262698,-2.,20.3994491700153));
#9085=CARTESIAN_POINT('',(-24.5395094084795,-4.,20.78429747225));
#9086=CARTESIAN_POINT('',(-24.3615406262698,-4.,20.3994491700153));
#9087=CARTESIAN_POINT('',(-24.5395094084795,-2.,20.78429747225));
#9088=CARTESIAN_POINT('Origin',(-18.3899090552018,-2.,24.3347446963989));
#9089=CARTESIAN_POINT('',(-24.5395094084795,-2.,20.78429747225));
#9090=CARTESIAN_POINT('',(-24.5395094084795,-4.,20.78429747225));
#9091=CARTESIAN_POINT('Origin',(-24.3615406262698,-2.,20.3994491700153));
#9092=CARTESIAN_POINT('',(-24.3615406262698,-2.,20.3994491700153));
#9093=CARTESIAN_POINT('',(-24.3615406262698,-4.,20.3994491700153));
#9094=CARTESIAN_POINT('Origin',(-32.3231572079194,-2.,39.2600978362433));
#9095=CARTESIAN_POINT('',(-32.405385595067,-2.,38.8441415939278));
#9096=CARTESIAN_POINT('',(-32.3231572079194,-2.,39.2600978362433));
#9097=CARTESIAN_POINT('',(-32.405385595067,-2.,38.8441415939278));
#9098=CARTESIAN_POINT('',(-32.405385595067,-4.,38.8441415939278));
#9099=CARTESIAN_POINT('',(-32.405385595067,-2.,38.8441415939278));
#9100=CARTESIAN_POINT('',(-32.3231572079194,-4.,39.2600978362433));
#9101=CARTESIAN_POINT('',(-32.405385595067,-4.,38.8441415939278));
#9102=CARTESIAN_POINT('',(-32.3231572079194,-2.,39.2600978362433));
#9103=CARTESIAN_POINT('Origin',(-25.2611254961061,-2.,38.517825583062));
#9104=CARTESIAN_POINT('',(-25.2611254961061,-2.,38.517825583062));
#9105=CARTESIAN_POINT('',(-32.3231572079194,-2.,39.2600978362433));
#9106=CARTESIAN_POINT('',(-25.2611254961061,-4.,38.517825583062));
#9107=CARTESIAN_POINT('',(-32.3231572079194,-4.,39.2600978362433));
#9108=CARTESIAN_POINT('',(-25.2611254961061,-2.,38.517825583062));
#9109=CARTESIAN_POINT('Origin',(-32.405385595067,-2.,38.8441415939278));
#9110=CARTESIAN_POINT('',(-24.8546847175204,-2.,36.2995923310118));
#9111=CARTESIAN_POINT('',(-32.405385595067,-2.,38.8441415939278));
#9112=CARTESIAN_POINT('',(-24.8546847175204,-4.,36.2995923310118));
#9113=CARTESIAN_POINT('',(-24.8546847175204,-2.,36.2995923310118));
#9114=CARTESIAN_POINT('',(-32.405385595067,-4.,38.8441415939278));
#9115=CARTESIAN_POINT('Origin',(5.11429163215176E-16,-2.,42.));
#9116=CARTESIAN_POINT('',(-25.4967316202476,-4.,41.5917394397366));
#9117=CARTESIAN_POINT('Origin',(5.11429163215176E-16,-4.,42.));
#9118=CARTESIAN_POINT('',(-25.4967316202476,-2.,41.5917394397366));
#9119=CARTESIAN_POINT('',(-25.4967316202476,-2.,41.5917394397366));
#9120=CARTESIAN_POINT('Origin',(5.11429163215176E-16,-2.,42.));
#9121=CARTESIAN_POINT('Origin',(5.11429163215176E-16,-2.,42.));
#9122=CARTESIAN_POINT('',(-23.9851245251038,-2.,33.3418361348804));
#9123=CARTESIAN_POINT('Origin',(5.11429163215176E-16,-2.,42.));
#9124=CARTESIAN_POINT('',(-23.9851245251038,-4.,33.3418361348804));
#9125=CARTESIAN_POINT('',(-23.9851245251038,-2.,33.3418361348804));
#9126=CARTESIAN_POINT('Origin',(5.11429163215176E-16,-4.,42.));
#9127=CARTESIAN_POINT('Origin',(-31.0471609795261,-2.,32.5996090046093));
#9128=CARTESIAN_POINT('',(-31.0411103134807,-2.,32.1756461611731));
#9129=CARTESIAN_POINT('',(-31.0471609795261,-2.,32.5996090046093));
#9130=CARTESIAN_POINT('',(-31.0411103134807,-2.,32.1756461611731));
#9131=CARTESIAN_POINT('',(-31.0411103134807,-4.,32.1756461611731));
#9132=CARTESIAN_POINT('',(-31.0411103134807,-2.,32.1756461611731));
#9133=CARTESIAN_POINT('',(-31.0471609795261,-4.,32.5996090046093));
#9134=CARTESIAN_POINT('',(-31.0411103134807,-4.,32.1756461611731));
#9135=CARTESIAN_POINT('',(-31.0471609795261,-2.,32.5996090046093));
#9136=CARTESIAN_POINT('Origin',(-23.9851245251038,-2.,33.3418361348804));
#9137=CARTESIAN_POINT('',(-31.0471609795261,-2.,32.5996090046093));
#9138=CARTESIAN_POINT('',(-31.0471609795261,-4.,32.5996090046093));
#9139=CARTESIAN_POINT('Origin',(-31.0411103134807,-2.,32.1756461611731));
#9140=CARTESIAN_POINT('',(-31.0411103134807,-2.,32.1756461611731));
#9141=CARTESIAN_POINT('',(-31.0411103134807,-4.,32.1756461611731));
#9142=CARTESIAN_POINT('Origin',(7.38260308224823,-2.,73.5878256213499));
#9143=CARTESIAN_POINT('',(7.01241515654905,-2.,73.7945670125629));
#9144=CARTESIAN_POINT('',(7.38260308224823,-2.,73.5878256213499));
#9145=CARTESIAN_POINT('',(7.01241515654905,-2.,73.7945670125629));
#9146=CARTESIAN_POINT('',(7.01241515654905,-4.,73.7945670125629));
#9147=CARTESIAN_POINT('',(7.01241515654905,-2.,73.7945670125629));
#9148=CARTESIAN_POINT('',(7.38260308224823,-4.,73.5878256213499));
#9149=CARTESIAN_POINT('',(7.01241515654905,-4.,73.7945670125629));
#9150=CARTESIAN_POINT('',(7.38260308224823,-2.,73.5878256213499));
#9151=CARTESIAN_POINT('Origin',(4.49437240522989,-2.,67.1008090842329));
#9152=CARTESIAN_POINT('',(4.49437240522989,-2.,67.1008090842329));
#9153=CARTESIAN_POINT('',(7.38260308224823,-2.,73.5878256213499));
#9154=CARTESIAN_POINT('',(4.49437240522989,-4.,67.1008090842329));
#9155=CARTESIAN_POINT('',(7.38260308224823,-4.,73.5878256213499));
#9156=CARTESIAN_POINT('',(4.49437240522989,-2.,67.1008090842329));
#9157=CARTESIAN_POINT('Origin',(7.01241515654905,-2.,73.7945670125629));
#9158=CARTESIAN_POINT('',(2.25911010841498,-2.,67.399732705642));
#9159=CARTESIAN_POINT('',(7.01241515654905,-2.,73.7945670125629));
#9160=CARTESIAN_POINT('',(2.25911010841498,-4.,67.399732705642));
#9161=CARTESIAN_POINT('',(2.25911010841497,-2.,67.399732705642));
#9162=CARTESIAN_POINT('',(7.01241515654905,-4.,73.7945670125629));
#9163=CARTESIAN_POINT('Origin',(5.11429163215176E-16,-2.,42.));
#9164=CARTESIAN_POINT('',(7.49064450548876,-4.,66.3749922029196));
#9165=CARTESIAN_POINT('Origin',(5.11429163215176E-16,-4.,42.));
#9166=CARTESIAN_POINT('',(7.49064450548876,-2.,66.3749922029196));
#9167=CARTESIAN_POINT('',(7.49064450548877,-2.,66.3749922029196));
#9168=CARTESIAN_POINT('Origin',(5.11429163215176E-16,-2.,42.));
#9169=CARTESIAN_POINT('Origin',(5.11429163215176E-16,-2.,42.));
#9170=CARTESIAN_POINT('',(-0.822592072616806,-2.,67.4867287481558));
#9171=CARTESIAN_POINT('Origin',(5.11429163215176E-16,-2.,42.));
#9172=CARTESIAN_POINT('',(-0.822592072616806,-4.,67.4867287481558));
#9173=CARTESIAN_POINT('',(-0.822592072616808,-2.,67.4867287481558));
#9174=CARTESIAN_POINT('Origin',(5.11429163215176E-16,-4.,42.));
#9175=CARTESIAN_POINT('Origin',(13.7887537262625,-2.,71.3626263544546));
#9176=CARTESIAN_POINT('',(13.4696392471283,-2.,71.6418163477944));
#9177=CARTESIAN_POINT('',(13.7887537262625,-2.,71.3626263544546));
#9178=CARTESIAN_POINT('',(13.4696392471283,-2.,71.6418163477944));
#9179=CARTESIAN_POINT('',(13.4696392471283,-4.,71.6418163477944));
#9180=CARTESIAN_POINT('',(13.4696392471283,-2.,71.6418163477944));
#9181=CARTESIAN_POINT('',(13.7887537262625,-4.,71.3626263544546));
#9182=CARTESIAN_POINT('',(13.4696392471283,-4.,71.6418163477944));
#9183=CARTESIAN_POINT('',(13.7887537262625,-2.,71.3626263544546));
#9184=CARTESIAN_POINT('Origin',(9.61491124257648,-2.,65.6178636162837));
#9185=CARTESIAN_POINT('',(13.7887537262625,-2.,71.3626263544546));
#9186=CARTESIAN_POINT('',(13.7887537262625,-4.,71.3626263544546));
#9187=CARTESIAN_POINT('Origin',(13.4696392471283,-2.,71.6418163477944));
#9188=CARTESIAN_POINT('',(13.4696392471283,-2.,71.6418163477944));
#9189=CARTESIAN_POINT('',(13.4696392471283,-4.,71.6418163477944));
#9190=CARTESIAN_POINT('Origin',(-18.5344034816569,-2.,68.622724190698));
#9191=CARTESIAN_POINT('',(-18.9357463479386,-2.,68.4859579417222));
#9192=CARTESIAN_POINT('',(-18.5344034816569,-2.,68.622724190698));
#9193=CARTESIAN_POINT('',(-18.9357463479386,-2.,68.4859579417222));
#9194=CARTESIAN_POINT('',(-18.9357463479386,-4.,68.4859579417222));
#9195=CARTESIAN_POINT('',(-18.9357463479386,-2.,68.4859579417222));
#9196=CARTESIAN_POINT('',(-18.5344034816569,-4.,68.622724190698));
#9197=CARTESIAN_POINT('',(-18.9357463479386,-4.,68.4859579417222));
#9198=CARTESIAN_POINT('',(-18.5344034816569,-2.,68.622724190698));
#9199=CARTESIAN_POINT('Origin',(-15.6462142535297,-2.,62.1356891993457));
#9200=CARTESIAN_POINT('',(-15.6462142535297,-2.,62.1356891993457));
#9201=CARTESIAN_POINT('',(-18.5344034816569,-2.,68.622724190698));
#9202=CARTESIAN_POINT('',(-15.6462142535297,-4.,62.1356891993457));
#9203=CARTESIAN_POINT('',(-18.5344034816569,-4.,68.622724190698));
#9204=CARTESIAN_POINT('',(-15.6462142535297,-2.,62.1356891993457));
#9205=CARTESIAN_POINT('Origin',(-18.9357463479386,-2.,68.4859579417222));
#9206=CARTESIAN_POINT('',(-17.3640402120316,-2.,60.6745845339314));
#9207=CARTESIAN_POINT('',(-18.9357463479386,-2.,68.4859579417222));
#9208=CARTESIAN_POINT('',(-17.3640402120316,-4.,60.6745845339314));
#9209=CARTESIAN_POINT('',(-17.3640402120316,-2.,60.6745845339314));
#9210=CARTESIAN_POINT('',(-18.9357463479386,-4.,68.4859579417222));
#9211=CARTESIAN_POINT('Origin',(5.11429163215176E-16,-2.,42.));
#9212=CARTESIAN_POINT('',(-13.1019298266752,-4.,63.8766870164767));
#9213=CARTESIAN_POINT('Origin',(5.11429163215176E-16,-4.,42.));
#9214=CARTESIAN_POINT('',(-13.1019298266752,-2.,63.8766870164767));
#9215=CARTESIAN_POINT('',(-13.1019298266752,-2.,63.8766870164767));
#9216=CARTESIAN_POINT('Origin',(5.11429163215176E-16,-2.,42.));
#9217=CARTESIAN_POINT('Origin',(5.11429163215176E-16,-2.,42.));
#9218=CARTESIAN_POINT('',(-19.490752119874,-2.,58.4426452191133));
#9219=CARTESIAN_POINT('Origin',(5.11429163215176E-16,-2.,42.));
#9220=CARTESIAN_POINT('',(-19.490752119874,-4.,58.4426452191133));
#9221=CARTESIAN_POINT('',(-19.490752119874,-2.,58.4426452191133));
#9222=CARTESIAN_POINT('Origin',(5.11429163215176E-16,-4.,42.));
#9223=CARTESIAN_POINT('Origin',(-12.5942066959522,-2.,71.8944729582989));
#9224=CARTESIAN_POINT('',(-13.0152145597486,-2.,71.8441392539282));
#9225=CARTESIAN_POINT('',(-12.5942066959522,-2.,71.8944729582989));
#9226=CARTESIAN_POINT('',(-13.0152145597486,-2.,71.8441392539282));
#9227=CARTESIAN_POINT('',(-13.0152145597486,-4.,71.8441392539282));
#9228=CARTESIAN_POINT('',(-13.0152145597486,-2.,71.8441392539282));
#9229=CARTESIAN_POINT('',(-12.5942066959522,-4.,71.8944729582989));
#9230=CARTESIAN_POINT('',(-13.0152145597486,-4.,71.8441392539282));
#9231=CARTESIAN_POINT('',(-12.5942066959522,-2.,71.8944729582989));
#9232=CARTESIAN_POINT('Origin',(-11.1178617454403,-2.,64.9487069398099));
#9233=CARTESIAN_POINT('',(-11.1178617454403,-2.,64.9487069398099));
#9234=CARTESIAN_POINT('',(-12.5942066959522,-2.,71.8944729582989));
#9235=CARTESIAN_POINT('',(-11.1178617454403,-4.,64.9487069398099));
#9236=CARTESIAN_POINT('',(-12.5942066959522,-4.,71.8944729582989));
#9237=CARTESIAN_POINT('',(-11.1178617454403,-2.,64.9487069398099));
#9238=CARTESIAN_POINT('Origin',(-13.0152145597486,-2.,71.8441392539282));
#9239=CARTESIAN_POINT('',(-13.0152145597486,-2.,71.8441392539282));
#9240=CARTESIAN_POINT('',(-13.0152145597486,-4.,71.8441392539282));
#9241=CARTESIAN_POINT('Origin',(5.11429163215176E-16,-2.,42.));
#9242=CARTESIAN_POINT('',(-8.26720223785845,-4.,66.1226733004107));
#9243=CARTESIAN_POINT('Origin',(5.11429163215176E-16,-4.,42.));
#9244=CARTESIAN_POINT('',(-8.26720223785845,-2.,66.1226733004107));
#9245=CARTESIAN_POINT('',(-8.26720223785845,-2.,66.1226733004107));
#9246=CARTESIAN_POINT('Origin',(5.11429163215176E-16,-2.,42.));
#9247=CARTESIAN_POINT('Origin',(-6.1035826439255,-2.,73.8596898080255));
#9248=CARTESIAN_POINT('',(-6.5258554413689,-2.,73.8979884726687));
#9249=CARTESIAN_POINT('',(-6.1035826439255,-2.,73.8596898080255));
#9250=CARTESIAN_POINT('',(-6.5258554413689,-2.,73.8979884726687));
#9251=CARTESIAN_POINT('',(-6.5258554413689,-4.,73.8979884726687));
#9252=CARTESIAN_POINT('',(-6.5258554413689,-2.,73.8979884726687));
#9253=CARTESIAN_POINT('',(-6.1035826439255,-4.,73.8596898080255));
#9254=CARTESIAN_POINT('',(-6.5258554413689,-4.,73.8979884726687));
#9255=CARTESIAN_POINT('',(-6.1035826439255,-2.,73.8596898080255));
#9256=CARTESIAN_POINT('Origin',(-6.10360532965543,-2.,66.7587560668908));
#9257=CARTESIAN_POINT('',(-6.10360532965543,-2.,66.7587560668908));
#9258=CARTESIAN_POINT('',(-6.1035826439255,-2.,73.8596898080255));
#9259=CARTESIAN_POINT('',(-6.10360532965543,-4.,66.7587560668908));
#9260=CARTESIAN_POINT('',(-6.1035826439255,-4.,73.8596898080255));
#9261=CARTESIAN_POINT('',(-6.10360532965543,-2.,66.7587560668908));
#9262=CARTESIAN_POINT('Origin',(-6.5258554413689,-2.,73.8979884726687));
#9263=CARTESIAN_POINT('',(-6.5258554413689,-2.,73.8979884726687));
#9264=CARTESIAN_POINT('',(-6.5258554413689,-4.,73.8979884726687));
#9265=CARTESIAN_POINT('Origin',(5.11429163215176E-16,-2.,42.));
#9266=CARTESIAN_POINT('',(-3.07115824080958,-4.,67.3143830076877));
#9267=CARTESIAN_POINT('Origin',(5.11429163215176E-16,-4.,42.));
#9268=CARTESIAN_POINT('',(-3.07115824080958,-2.,67.3143830076877));
#9269=CARTESIAN_POINT('',(-3.07115824080957,-2.,67.3143830076877));
#9270=CARTESIAN_POINT('Origin',(5.11429163215176E-16,-2.,42.));
#9271=CARTESIAN_POINT('Origin',(-23.6645578972779,-2.,64.1874346259592));
#9272=CARTESIAN_POINT('',(-24.0286951569316,-2.,63.9702131737359));
#9273=CARTESIAN_POINT('',(-23.6645578972779,-2.,64.1874346259592));
#9274=CARTESIAN_POINT('',(-24.0286951569316,-2.,63.9702131737359));
#9275=CARTESIAN_POINT('',(-24.0286951569316,-4.,63.9702131737359));
#9276=CARTESIAN_POINT('',(-24.0286951569316,-2.,63.9702131737359));
#9277=CARTESIAN_POINT('',(-23.6645578972779,-4.,64.1874346259592));
#9278=CARTESIAN_POINT('',(-24.0286951569316,-4.,63.9702131737359));
#9279=CARTESIAN_POINT('',(-23.6645578972779,-2.,64.1874346259592));
#9280=CARTESIAN_POINT('Origin',(-19.490752119874,-2.,58.4426452191133));
#9281=CARTESIAN_POINT('',(-23.6645578972779,-2.,64.1874346259592));
#9282=CARTESIAN_POINT('',(-23.6645578972779,-4.,64.1874346259592));
#9283=CARTESIAN_POINT('Origin',(-24.0286951569316,-2.,63.9702131737359));
#9284=CARTESIAN_POINT('',(-20.8672587182129,-2.,56.6563130966546));
#9285=CARTESIAN_POINT('',(-24.0286951569316,-2.,63.9702131737359));
#9286=CARTESIAN_POINT('',(-20.8672587182129,-4.,56.6563130966546));
#9287=CARTESIAN_POINT('',(-20.8672587182129,-2.,56.6563130966546));
#9288=CARTESIAN_POINT('',(-24.0286951569316,-4.,63.9702131737359));
#9289=CARTESIAN_POINT('Origin',(5.11429163215176E-16,-2.,42.));
#9290=CARTESIAN_POINT('',(-22.4834505915744,-2.,54.03097874224));
#9291=CARTESIAN_POINT('Origin',(5.11429163215176E-16,-2.,42.));
#9292=CARTESIAN_POINT('',(-22.4834505915744,-4.,54.03097874224));
#9293=CARTESIAN_POINT('',(-22.4834505915744,-2.,54.03097874224));
#9294=CARTESIAN_POINT('Origin',(5.11429163215176E-16,-4.,42.));
#9295=CARTESIAN_POINT('Origin',(-30.643092052405,-2.,52.6439872802755));
#9296=CARTESIAN_POINT('',(-30.8873960676387,-2.,52.297437642684));
#9297=CARTESIAN_POINT('',(-30.643092052405,-2.,52.6439872802755));
#9298=CARTESIAN_POINT('',(-30.8873960676387,-2.,52.297437642684));
#9299=CARTESIAN_POINT('',(-30.8873960676387,-4.,52.297437642684));
#9300=CARTESIAN_POINT('',(-30.8873960676387,-2.,52.297437642684));
#9301=CARTESIAN_POINT('',(-30.643092052405,-4.,52.6439872802755));
#9302=CARTESIAN_POINT('',(-30.8873960676387,-4.,52.297437642684));
#9303=CARTESIAN_POINT('',(-30.643092052405,-2.,52.6439872802755));
#9304=CARTESIAN_POINT('Origin',(-24.4935143848573,-2.,49.0935007632897));
#9305=CARTESIAN_POINT('',(-24.4935143848573,-2.,49.0935007632897));
#9306=CARTESIAN_POINT('',(-30.643092052405,-2.,52.6439872802755));
#9307=CARTESIAN_POINT('',(-24.4935143848573,-4.,49.0935007632897));
#9308=CARTESIAN_POINT('',(-30.643092052405,-4.,52.6439872802755));
#9309=CARTESIAN_POINT('',(-24.4935143848572,-2.,49.0935007632897));
#9310=CARTESIAN_POINT('Origin',(-30.8873960676387,-2.,52.297437642684));
#9311=CARTESIAN_POINT('',(-25.0244490042775,-2.,46.9017294939964));
#9312=CARTESIAN_POINT('',(-30.8873960676387,-2.,52.297437642684));
#9313=CARTESIAN_POINT('',(-25.0244490042775,-4.,46.9017294939964));
#9314=CARTESIAN_POINT('',(-25.0244490042775,-2.,46.9017294939964));
#9315=CARTESIAN_POINT('',(-30.8873960676387,-4.,52.297437642684));
#9316=CARTESIAN_POINT('Origin',(5.11429163215176E-16,-2.,42.));
#9317=CARTESIAN_POINT('',(-23.4584778861915,-4.,51.9974904482608));
#9318=CARTESIAN_POINT('Origin',(5.11429163215176E-16,-4.,42.));
#9319=CARTESIAN_POINT('',(-23.4584778861915,-2.,51.9974904482608));
#9320=CARTESIAN_POINT('',(-23.4584778861915,-2.,51.9974904482608));
#9321=CARTESIAN_POINT('Origin',(5.11429163215176E-16,-2.,42.));
#9322=CARTESIAN_POINT('Origin',(5.11429163215176E-16,-2.,42.));
#9323=CARTESIAN_POINT('',(-25.4330940665997,-2.,43.8460027625905));
#9324=CARTESIAN_POINT('Origin',(5.11429163215176E-16,-2.,42.));
#9325=CARTESIAN_POINT('',(-25.4330940665997,-4.,43.8460027625905));
#9326=CARTESIAN_POINT('',(-25.4330940665997,-2.,43.8460027625905));
#9327=CARTESIAN_POINT('Origin',(5.11429163215176E-16,-4.,42.));
#9328=CARTESIAN_POINT('Origin',(-27.7604575776403,-2.,58.7824477009424));
#9329=CARTESIAN_POINT('',(-28.0714746850947,-2.,58.4942646652779));
#9330=CARTESIAN_POINT('',(-27.7604575776403,-2.,58.7824477009424));
#9331=CARTESIAN_POINT('',(-28.0714746850947,-2.,58.4942646652779));
#9332=CARTESIAN_POINT('',(-28.0714746850947,-4.,58.4942646652779));
#9333=CARTESIAN_POINT('',(-28.0714746850947,-2.,58.4942646652779));
#9334=CARTESIAN_POINT('',(-27.7604575776403,-4.,58.7824477009424));
#9335=CARTESIAN_POINT('',(-28.0714746850947,-4.,58.4942646652779));
#9336=CARTESIAN_POINT('',(-27.7604575776403,-2.,58.7824477009424));
#9337=CARTESIAN_POINT('Origin',(-22.4834505915744,-2.,54.03097874224));
#9338=CARTESIAN_POINT('',(-27.7604575776403,-2.,58.7824477009424));
#9339=CARTESIAN_POINT('',(-27.7604575776403,-4.,58.7824477009424));
#9340=CARTESIAN_POINT('Origin',(-28.0714746850947,-2.,58.4942646652779));
#9341=CARTESIAN_POINT('',(-28.0714746850947,-2.,58.4942646652779));
#9342=CARTESIAN_POINT('',(-28.0714746850947,-4.,58.4942646652779));
#9343=CARTESIAN_POINT('Origin',(-32.1864763626099,-2.,46.0403335399428));
#9344=CARTESIAN_POINT('',(-32.3533900278565,-2.,45.6505631825167));
#9345=CARTESIAN_POINT('',(-32.1864763626099,-2.,46.0403335399428));
#9346=CARTESIAN_POINT('',(-32.3533900278565,-2.,45.6505631825167));
#9347=CARTESIAN_POINT('',(-32.3533900278565,-4.,45.6505631825167));
#9348=CARTESIAN_POINT('',(-32.3533900278565,-2.,45.6505631825167));
#9349=CARTESIAN_POINT('',(-32.1864763626099,-4.,46.0403335399428));
#9350=CARTESIAN_POINT('',(-32.3533900278565,-4.,45.6505631825167));
#9351=CARTESIAN_POINT('',(-32.1864763626099,-2.,46.0403335399428));
#9352=CARTESIAN_POINT('Origin',(-25.4330940665997,-2.,43.8460027625905));
#9353=CARTESIAN_POINT('',(-32.1864763626099,-2.,46.0403335399428));
#9354=CARTESIAN_POINT('',(-32.1864763626099,-4.,46.0403335399428));
#9355=CARTESIAN_POINT('Origin',(-32.3533900278565,-2.,45.6505631825167));
#9356=CARTESIAN_POINT('',(-32.3533900278565,-2.,45.6505631825167));
#9357=CARTESIAN_POINT('',(-32.3533900278565,-4.,45.6505631825167));
#9358=CARTESIAN_POINT('Origin',(0.653797257879684,-2.,74.4324853333879));
#9359=CARTESIAN_POINT('',(0.248714874327309,-2.,74.5577425316228));
#9360=CARTESIAN_POINT('',(0.653797257879684,-2.,74.4324853333879));
#9361=CARTESIAN_POINT('',(0.248714874327309,-2.,74.5577425316228));
#9362=CARTESIAN_POINT('',(0.248714874327309,-4.,74.5577425316228));
#9363=CARTESIAN_POINT('',(0.248714874327309,-2.,74.5577425316228));
#9364=CARTESIAN_POINT('',(0.653797257879684,-4.,74.4324853333879));
#9365=CARTESIAN_POINT('',(0.248714874327309,-4.,74.5577425316228));
#9366=CARTESIAN_POINT('',(0.653797257879684,-2.,74.4324853333879));
#9367=CARTESIAN_POINT('Origin',(-0.822592072616806,-2.,67.4867287481558));
#9368=CARTESIAN_POINT('',(0.653797257879684,-2.,74.4324853333879));
#9369=CARTESIAN_POINT('',(0.653797257879684,-4.,74.4324853333879));
#9370=CARTESIAN_POINT('Origin',(0.248714874327309,-2.,74.5577425316228));
#9371=CARTESIAN_POINT('',(0.248714874327309,-2.,74.5577425316228));
#9372=CARTESIAN_POINT('',(0.248714874327309,-4.,74.5577425316228));
#9373=CARTESIAN_POINT('Origin',(21.9692735008546,-2.,43.1623346526058));
#9374=CARTESIAN_POINT('',(6.705461117593,-2.,44.0091767469411));
#9375=CARTESIAN_POINT('',(21.9692735008546,-2.,43.1623346526058));
#9376=CARTESIAN_POINT('',(6.705461117593,-2.,44.0091767469411));
#9377=CARTESIAN_POINT('',(6.705461117593,-4.,44.0091767469411));
#9378=CARTESIAN_POINT('',(6.70546111759299,-2.,44.0091767469411));
#9379=CARTESIAN_POINT('',(21.9692735008546,-4.,43.1623346526058));
#9380=CARTESIAN_POINT('',(6.705461117593,-4.,44.0091767469411));
#9381=CARTESIAN_POINT('',(21.9692735008546,-2.,43.1623346526058));
#9382=CARTESIAN_POINT('Origin',(6.705461117593,-2.,39.9908232530589));
#9383=CARTESIAN_POINT('',(6.705461117593,-2.,39.9908232530589));
#9384=CARTESIAN_POINT('',(21.9692735008546,-2.,40.8376653473942));
#9385=CARTESIAN_POINT('',(6.705461117593,-2.,39.9908232530589));
#9386=CARTESIAN_POINT('',(21.9692735008546,-4.,40.8376653473942));
#9387=CARTESIAN_POINT('',(21.9692735008546,-2.,40.8376653473942));
#9388=CARTESIAN_POINT('',(6.705461117593,-4.,39.9908232530589));
#9389=CARTESIAN_POINT('',(6.705461117593,-4.,39.9908232530589));
#9390=CARTESIAN_POINT('',(6.705461117593,-2.,39.9908232530589));
#9391=CARTESIAN_POINT('Origin',(5.11429163215176E-16,-2.,42.));
#9392=CARTESIAN_POINT('',(11.9912480872829,-4.,60.4447816281255));
#9393=CARTESIAN_POINT('Origin',(5.11429163215176E-16,-4.,42.));
#9394=CARTESIAN_POINT('',(11.9912480872829,-2.,60.4447816281255));
#9395=CARTESIAN_POINT('',(11.9912480872829,-2.,60.4447816281255));
#9396=CARTESIAN_POINT('Origin',(5.11429163215176E-16,-2.,42.));
#9397=CARTESIAN_POINT('Origin',(5.11429163215176E-16,-2.,42.));
#9398=CARTESIAN_POINT('',(11.9912480872829,-2.,23.5552183718745));
#9399=CARTESIAN_POINT('Origin',(5.11429163215176E-16,-2.,42.));
#9400=CARTESIAN_POINT('',(11.9912480872829,-4.,23.5552183718745));
#9401=CARTESIAN_POINT('',(11.9912480872829,-2.,23.5552183718745));
#9402=CARTESIAN_POINT('Origin',(5.11429163215176E-16,-4.,42.));
#9403=CARTESIAN_POINT('Origin',(5.11429163215176E-16,-2.,42.));
#9404=CARTESIAN_POINT('',(5.09272866234044,-4.,37.1974887015462));
#9405=CARTESIAN_POINT('Origin',(5.11429163215176E-16,-4.,42.));
#9406=CARTESIAN_POINT('',(5.09272866234044,-2.,37.1974887015462));
#9407=CARTESIAN_POINT('',(5.09272866234044,-2.,37.1974887015462));
#9408=CARTESIAN_POINT('Origin',(5.11429163215176E-16,-2.,42.));
#9409=CARTESIAN_POINT('Origin',(5.11429163215176E-16,-2.,42.));
#9410=CARTESIAN_POINT('',(5.09272866234043,-2.,46.8025112984538));
#9411=CARTESIAN_POINT('Origin',(5.11429163215176E-16,-2.,42.));
#9412=CARTESIAN_POINT('',(5.09272866234043,-4.,46.8025112984538));
#9413=CARTESIAN_POINT('',(5.09272866234043,-2.,46.8025112984538));
#9414=CARTESIAN_POINT('Origin',(5.11429163215176E-16,-4.,42.));
#9415=CARTESIAN_POINT('Origin',(11.9912480872829,-2.,23.5552183718745));
#9416=CARTESIAN_POINT('',(5.09272866234044,-2.,37.1974887015462));
#9417=CARTESIAN_POINT('',(5.09272866234044,-4.,37.1974887015462));
#9418=CARTESIAN_POINT('Origin',(1.61273245525256,-2.,35.1883119546051));
#9419=CARTESIAN_POINT('',(1.61273245525256,-2.,35.1883119546051));
#9420=CARTESIAN_POINT('',(9.97802541357168,-2.,22.3928837192687));
#9421=CARTESIAN_POINT('',(1.61273245525256,-2.,35.1883119546051));
#9422=CARTESIAN_POINT('',(9.97802541357168,-4.,22.3928837192687));
#9423=CARTESIAN_POINT('',(9.97802541357168,-2.,22.3928837192687));
#9424=CARTESIAN_POINT('',(1.61273245525256,-4.,35.1883119546051));
#9425=CARTESIAN_POINT('',(1.61273245525256,-4.,35.1883119546051));
#9426=CARTESIAN_POINT('',(1.61273245525256,-2.,35.1883119546051));
#9427=CARTESIAN_POINT('Origin',(5.11429163215176E-16,-2.,42.));
#9428=CARTESIAN_POINT('',(-9.97802541357168,-2.,22.3928837192687));
#9429=CARTESIAN_POINT('Origin',(5.11429163215176E-16,-2.,42.));
#9430=CARTESIAN_POINT('',(-9.97802541357168,-4.,22.3928837192687));
#9431=CARTESIAN_POINT('',(-9.97802541357167,-2.,22.3928837192687));
#9432=CARTESIAN_POINT('Origin',(5.11429163215176E-16,-4.,42.));
#9433=CARTESIAN_POINT('Origin',(5.11429163215176E-16,-2.,42.));
#9434=CARTESIAN_POINT('',(-1.61273245525256,-4.,35.1883119546051));
#9435=CARTESIAN_POINT('Origin',(5.11429163215176E-16,-4.,42.));
#9436=CARTESIAN_POINT('',(-1.61273245525256,-2.,35.1883119546051));
#9437=CARTESIAN_POINT('',(-1.61273245525255,-2.,35.1883119546051));
#9438=CARTESIAN_POINT('Origin',(5.11429163215176E-16,-2.,42.));
#9439=CARTESIAN_POINT('Origin',(-9.97802541357168,-2.,22.3928837192687));
#9440=CARTESIAN_POINT('',(-1.61273245525256,-2.,35.1883119546051));
#9441=CARTESIAN_POINT('',(-1.61273245525256,-4.,35.1883119546051));
#9442=CARTESIAN_POINT('Origin',(-5.09272866234044,-2.,37.1974887015462));
#9443=CARTESIAN_POINT('',(-5.09272866234044,-2.,37.1974887015462));
#9444=CARTESIAN_POINT('',(-11.9912480872829,-2.,23.5552183718745));
#9445=CARTESIAN_POINT('',(-5.09272866234044,-2.,37.1974887015462));
#9446=CARTESIAN_POINT('',(-11.9912480872829,-4.,23.5552183718745));
#9447=CARTESIAN_POINT('',(-11.9912480872829,-2.,23.5552183718745));
#9448=CARTESIAN_POINT('',(-5.09272866234044,-4.,37.1974887015462));
#9449=CARTESIAN_POINT('',(-5.09272866234044,-4.,37.1974887015462));
#9450=CARTESIAN_POINT('',(-5.09272866234043,-2.,37.1974887015462));
#9451=CARTESIAN_POINT('Origin',(5.11429163215176E-16,-2.,42.));
#9452=CARTESIAN_POINT('',(-21.9692735008546,-2.,40.8376653473942));
#9453=CARTESIAN_POINT('Origin',(5.11429163215176E-16,-2.,42.));
#9454=CARTESIAN_POINT('',(-21.9692735008546,-4.,40.8376653473942));
#9455=CARTESIAN_POINT('',(-21.9692735008546,-2.,40.8376653473942));
#9456=CARTESIAN_POINT('Origin',(5.11429163215176E-16,-4.,42.));
#9457=CARTESIAN_POINT('Origin',(5.11429163215176E-16,-2.,42.));
#9458=CARTESIAN_POINT('',(-6.705461117593,-4.,39.9908232530589));
#9459=CARTESIAN_POINT('Origin',(5.11429163215176E-16,-4.,42.));
#9460=CARTESIAN_POINT('',(-6.705461117593,-2.,39.9908232530589));
#9461=CARTESIAN_POINT('',(-6.70546111759299,-2.,39.9908232530589));
#9462=CARTESIAN_POINT('Origin',(5.11429163215176E-16,-2.,42.));
#9463=CARTESIAN_POINT('Origin',(-21.9692735008546,-2.,40.8376653473942));
#9464=CARTESIAN_POINT('',(-6.705461117593,-2.,39.9908232530589));
#9465=CARTESIAN_POINT('',(-6.705461117593,-4.,39.9908232530589));
#9466=CARTESIAN_POINT('Origin',(-6.705461117593,-2.,44.0091767469411));
#9467=CARTESIAN_POINT('',(-6.705461117593,-2.,44.0091767469411));
#9468=CARTESIAN_POINT('',(-21.9692735008546,-2.,43.1623346526058));
#9469=CARTESIAN_POINT('',(-6.705461117593,-2.,44.0091767469411));
#9470=CARTESIAN_POINT('',(-21.9692735008546,-4.,43.1623346526058));
#9471=CARTESIAN_POINT('',(-21.9692735008546,-2.,43.1623346526058));
#9472=CARTESIAN_POINT('',(-6.705461117593,-4.,44.0091767469411));
#9473=CARTESIAN_POINT('',(-6.705461117593,-4.,44.0091767469411));
#9474=CARTESIAN_POINT('',(-6.70546111759299,-2.,44.0091767469411));
#9475=CARTESIAN_POINT('Origin',(5.11429163215176E-16,-2.,42.));
#9476=CARTESIAN_POINT('',(-11.9912480872829,-2.,60.4447816281255));
#9477=CARTESIAN_POINT('Origin',(5.11429163215176E-16,-2.,42.));
#9478=CARTESIAN_POINT('',(-11.9912480872829,-4.,60.4447816281255));
#9479=CARTESIAN_POINT('',(-11.9912480872829,-2.,60.4447816281255));
#9480=CARTESIAN_POINT('Origin',(5.11429163215176E-16,-4.,42.));
#9481=CARTESIAN_POINT('Origin',(5.11429163215176E-16,-2.,42.));
#9482=CARTESIAN_POINT('',(-5.09272866234044,-4.,46.8025112984538));
#9483=CARTESIAN_POINT('Origin',(5.11429163215176E-16,-4.,42.));
#9484=CARTESIAN_POINT('',(-5.09272866234044,-2.,46.8025112984538));
#9485=CARTESIAN_POINT('',(-5.09272866234044,-2.,46.8025112984538));
#9486=CARTESIAN_POINT('Origin',(5.11429163215176E-16,-2.,42.));
#9487=CARTESIAN_POINT('Origin',(-11.9912480872829,-2.,60.4447816281255));
#9488=CARTESIAN_POINT('',(-5.09272866234044,-2.,46.8025112984538));
#9489=CARTESIAN_POINT('',(-5.09272866234044,-4.,46.8025112984538));
#9490=CARTESIAN_POINT('Origin',(-1.61273245525257,-2.,48.8116880453949));
#9491=CARTESIAN_POINT('',(-1.61273245525257,-2.,48.8116880453949));
#9492=CARTESIAN_POINT('',(-9.97802541357169,-2.,61.6071162807313));
#9493=CARTESIAN_POINT('',(-1.61273245525257,-2.,48.8116880453949));
#9494=CARTESIAN_POINT('',(-9.97802541357169,-4.,61.6071162807313));
#9495=CARTESIAN_POINT('',(-9.97802541357169,-2.,61.6071162807313));
#9496=CARTESIAN_POINT('',(-1.61273245525257,-4.,48.8116880453949));
#9497=CARTESIAN_POINT('',(-1.61273245525257,-4.,48.8116880453949));
#9498=CARTESIAN_POINT('',(-1.61273245525256,-2.,48.8116880453949));
#9499=CARTESIAN_POINT('Origin',(5.11429163215176E-16,-2.,42.));
#9500=CARTESIAN_POINT('',(9.97802541357166,-2.,61.6071162807313));
#9501=CARTESIAN_POINT('Origin',(5.11429163215176E-16,-2.,42.));
#9502=CARTESIAN_POINT('',(9.97802541357166,-4.,61.6071162807313));
#9503=CARTESIAN_POINT('',(9.97802541357166,-2.,61.6071162807313));
#9504=CARTESIAN_POINT('Origin',(5.11429163215176E-16,-4.,42.));
#9505=CARTESIAN_POINT('Origin',(5.11429163215176E-16,-2.,42.));
#9506=CARTESIAN_POINT('',(1.61273245525255,-4.,48.8116880453949));
#9507=CARTESIAN_POINT('Origin',(5.11429163215176E-16,-4.,42.));
#9508=CARTESIAN_POINT('',(1.61273245525255,-2.,48.8116880453949));
#9509=CARTESIAN_POINT('',(1.61273245525255,-2.,48.8116880453949));
#9510=CARTESIAN_POINT('Origin',(5.11429163215176E-16,-2.,42.));
#9511=CARTESIAN_POINT('Origin',(9.97802541357166,-2.,61.6071162807313));
#9512=CARTESIAN_POINT('',(1.61273245525255,-2.,48.8116880453949));
#9513=CARTESIAN_POINT('',(1.61273245525255,-4.,48.8116880453949));
#9514=CARTESIAN_POINT('Origin',(5.09272866234043,-2.,46.8025112984538));
#9515=CARTESIAN_POINT('',(5.09272866234043,-2.,46.8025112984538));
#9516=CARTESIAN_POINT('',(5.09272866234043,-4.,46.8025112984538));
#9517=CARTESIAN_POINT('Origin',(5.11429163215176E-16,-2.,42.));
#9518=CARTESIAN_POINT('',(-6.00000000000001,-2.,42.));
#9519=CARTESIAN_POINT('Origin',(5.11429163215176E-16,-2.,42.));
#9520=CARTESIAN_POINT('',(-6.00000000000001,-4.,42.));
#9521=CARTESIAN_POINT('',(-6.00000000000001,-2.,42.));
#9522=CARTESIAN_POINT('Origin',(5.11429163215176E-16,-4.,42.));
#9523=CARTESIAN_POINT('Origin',(0.,-4.,42.));
#9524=CARTESIAN_POINT('Origin',(0.,-2.,42.));
#9525=CARTESIAN_POINT('',(0.,0.,0.));
#9526=CARTESIAN_POINT('Origin',(3.64981768126446E-16,-4.,86.8));
#9527=CARTESIAN_POINT('',(-3.37715398312954,-4.,86.8));
#9528=CARTESIAN_POINT('Origin',(3.64981768126446E-16,-4.,86.8));
#9529=CARTESIAN_POINT('',(-3.37715398312954,-4.5,86.8));
#9530=CARTESIAN_POINT('',(-3.37715398312954,-4.,86.8));
#9531=CARTESIAN_POINT('Origin',(3.64981768126446E-16,-4.5,86.8));
#9532=CARTESIAN_POINT('Origin',(0.637540569301853,-4.,78.5706101655767));
#9533=CARTESIAN_POINT('',(-6.00000000000001,-4.,86.8));
#9534=CARTESIAN_POINT('Origin',(5.11429163215176E-16,-4.,86.8));
#9535=CARTESIAN_POINT('Origin',(0.637540569301853,-4.5,78.5706101655767));
#9536=CARTESIAN_POINT('',(-23.8080041831819,-4.5,69.5119859113367));
#9537=CARTESIAN_POINT('',(-16.7912595803416,-4.5,73.6727335932742));
#9538=CARTESIAN_POINT('',(-23.8080041831819,-4.5,69.5119859113367));
#9539=CARTESIAN_POINT('',(-16.8211392806367,-4.5,73.7231231486636));
#9540=CARTESIAN_POINT('',(-16.7912595803416,-4.5,73.6727335932742));
#9541=CARTESIAN_POINT('',(-4.20530738557349,-4.5,81.2039844717119));
#9542=CARTESIAN_POINT('',(-16.8211392806367,-4.5,73.7231231486636));
#9543=CARTESIAN_POINT('',(4.87558269014984,-4.5,81.777182719677));
#9544=CARTESIAN_POINT('Origin',(5.11429163215176E-16,-4.5,86.8));
#9545=CARTESIAN_POINT('',(25.14540508495,-4.5,70.6940477528968));
#9546=CARTESIAN_POINT('',(4.87558269014983,-4.5,81.777182719677));
#9547=CARTESIAN_POINT('',(22.0328538621538,-4.5,66.4556698663697));
#9548=CARTESIAN_POINT('Origin',(0.298639064659696,-4.5,85.6787712833559));
#9549=CARTESIAN_POINT('',(23.5123684627238,-4.5,63.3412203311535));
#9550=CARTESIAN_POINT('',(22.0328538621538,-4.5,66.4556698663697));
#9551=CARTESIAN_POINT('',(29.4580576969316,-4.5,71.983088746998));
#9552=CARTESIAN_POINT('Origin',(0.298639064659696,-4.5,85.6787712833559));
#9553=CARTESIAN_POINT('',(6.60407749680247,-4.5,84.4791897069714));
#9554=CARTESIAN_POINT('',(29.4580576969316,-4.5,71.983088746998));
#9555=CARTESIAN_POINT('',(-6.27473995448561,-4.5,83.6971563842852));
#9556=CARTESIAN_POINT('Origin',(5.11429163215176E-16,-4.5,86.8));
#9557=CARTESIAN_POINT('',(-19.225775115544,-4.5,76.0175282126611));
#9558=CARTESIAN_POINT('',(-6.27473995448561,-4.5,83.6971563842852));
#9559=CARTESIAN_POINT('',(-19.1958954152489,-4.5,75.9671386572717));
#9560=CARTESIAN_POINT('',(-19.225775115544,-4.5,76.0175282126611));
#9561=CARTESIAN_POINT('',(-28.1829765583279,-4.5,70.6380324762781));
#9562=CARTESIAN_POINT('',(-19.1958954152489,-4.5,75.9671386572717));
#9563=CARTESIAN_POINT('',(-22.8617076926603,-4.5,63.4624614786761));
#9564=CARTESIAN_POINT('Origin',(-4.36669271088479,-4.5,82.738879784617));
#9565=CARTESIAN_POINT('',(-19.6350203672456,-4.5,64.8561091973757));
#9566=CARTESIAN_POINT('',(-22.8617076926603,-4.5,63.4624614786761));
#9567=CARTESIAN_POINT('Origin',(-4.36669271088479,-4.5,82.738879784617));
#9568=CARTESIAN_POINT('Origin',(-18.4234042975864,-2.,76.4252058677884));
#9569=CARTESIAN_POINT('',(-16.8211392806367,-2.,73.7231231486636));
#9570=CARTESIAN_POINT('',(-16.8211392806367,-2.,73.7231231486636));
#9571=CARTESIAN_POINT('',(-16.7912595803416,-2.,73.6727335932742));
#9572=CARTESIAN_POINT('',(-16.7912595803416,-2.,73.6727335932742));
#9573=CARTESIAN_POINT('',(-16.4205260287817,-2.,73.0475232114257));
#9574=CARTESIAN_POINT('Origin',(-4.36669271088479,-2.,82.738879784617));
#9575=CARTESIAN_POINT('',(-28.1829765583279,-2.,70.6380324762781));
#9576=CARTESIAN_POINT('',(-22.8617076926605,-2.,63.4624614786759));
#9577=CARTESIAN_POINT('Origin',(-4.36669271088479,-2.,82.738879784617));
#9578=CARTESIAN_POINT('',(-22.8617076926605,-2.,63.4624614786759));
#9579=CARTESIAN_POINT('',(-28.1829765583279,-2.,70.6380324762781));
#9580=CARTESIAN_POINT('Origin',(-22.8617076926605,-2.,63.4624614786759));
#9581=CARTESIAN_POINT('',(-19.6350203672463,-2.,64.8561091973748));
#9582=CARTESIAN_POINT('',(-22.8617076926605,-2.,63.4624614786759));
#9583=CARTESIAN_POINT('',(-19.6350203672463,-2.,64.8561091973748));
#9584=CARTESIAN_POINT('Origin',(-4.36669271088479,-2.,82.738879784617));
#9585=CARTESIAN_POINT('',(-23.808004183182,-2.,69.5119859113367));
#9586=CARTESIAN_POINT('Origin',(-4.36669271088479,-2.,82.738879784617));
#9587=CARTESIAN_POINT('',(-23.808004183182,-2.,69.5119859113367));
#9588=CARTESIAN_POINT('Origin',(-5.47236913652802,-2.,84.1048340394125));
#9589=CARTESIAN_POINT('',(-19.1958954152489,-2.,75.9671386572717));
#9590=CARTESIAN_POINT('',(-19.1958954152489,-2.,75.9671386572717));
#9591=CARTESIAN_POINT('',(-31.1673936222204,-2.,68.8683505107269));
#9592=CARTESIAN_POINT('Origin',(-23.808004183182,-2.,69.5119859113367));
#9593=CARTESIAN_POINT('',(-29.5352489049756,-2.,66.1158782362127));
#9594=CARTESIAN_POINT('Origin',(0.236355160323063,-2.,78.4273919117743));
#9595=CARTESIAN_POINT('',(-19.225775115544,-2.,76.0175282126611));
#9596=CARTESIAN_POINT('',(-17.2228968467393,-2.,72.6398455562984));
#9597=CARTESIAN_POINT('',(-6.2747399544856,-2.,83.6971563842852));
#9598=CARTESIAN_POINT('',(-31.969764440178,-2.,68.4606728555997));
#9599=CARTESIAN_POINT('',(6.60407749680247,-2.,84.4791897069714));
#9600=CARTESIAN_POINT('Origin',(5.11429163215176E-16,-2.,86.8));
#9601=CARTESIAN_POINT('',(29.4580576969316,-2.,71.983088746998));
#9602=CARTESIAN_POINT('',(6.60407749680247,-2.,84.4791897069714));
#9603=CARTESIAN_POINT('',(23.5123684627238,-2.,63.3412203311535));
#9604=CARTESIAN_POINT('Origin',(0.29863906465954,-2.,85.678771283356));
#9605=CARTESIAN_POINT('',(22.0328538621538,-2.,66.4556698663697));
#9606=CARTESIAN_POINT('',(22.0328538621538,-2.,66.4556698663697));
#9607=CARTESIAN_POINT('',(25.14540508495,-2.,70.6940477528968));
#9608=CARTESIAN_POINT('Origin',(0.29863906465954,-2.,85.678771283356));
#9609=CARTESIAN_POINT('',(4.87558269014984,-2.,81.777182719677));
#9610=CARTESIAN_POINT('',(4.87558269014984,-2.,81.777182719677));
#9611=CARTESIAN_POINT('',(-4.20530738557349,-2.,81.2039844717119));
#9612=CARTESIAN_POINT('Origin',(5.11429163215176E-16,-2.,86.8));
#9613=CARTESIAN_POINT('',(-30.3376197229332,-2.,65.7082005810854));
#9614=CARTESIAN_POINT('',(-6.00000000000001,-2.,86.8));
#9615=CARTESIAN_POINT('Origin',(5.11429163215176E-16,-2.,86.8));
#9616=CARTESIAN_POINT('Origin',(-19.225775115544,-2.,76.0175282126611));
#9617=CARTESIAN_POINT('',(-19.225775115544,-2.,76.0175282126611));
#9618=CARTESIAN_POINT('Origin',(-6.2747399544856,-2.,83.6971563842852));
#9619=CARTESIAN_POINT('',(-6.2747399544856,-2.,83.6971563842852));
#9620=CARTESIAN_POINT('Origin',(5.11429163215176E-16,-2.,86.8));
#9621=CARTESIAN_POINT('',(-6.00000000000001,-2.,86.8));
#9622=CARTESIAN_POINT('Origin',(5.11429163215176E-16,-2.,86.8));
#9623=CARTESIAN_POINT('',(6.60407749680247,-2.,84.4791897069714));
#9624=CARTESIAN_POINT('Origin',(29.4580576969316,-2.,71.983088746998));
#9625=CARTESIAN_POINT('',(29.4580576969316,-2.,71.983088746998));
#9626=CARTESIAN_POINT('Origin',(0.29863906465954,-2.,85.678771283356));
#9627=CARTESIAN_POINT('',(23.5123684627238,-2.,63.3412203311535));
#9628=CARTESIAN_POINT('Origin',(22.0328538621538,-2.,66.4556698663697));
#9629=CARTESIAN_POINT('',(22.0328538621538,-2.,66.4556698663697));
#9630=CARTESIAN_POINT('Origin',(0.29863906465954,-2.,85.678771283356));
#9631=CARTESIAN_POINT('',(25.14540508495,-2.,70.6940477528968));
#9632=CARTESIAN_POINT('Origin',(4.87558269014984,-2.,81.777182719677));
#9633=CARTESIAN_POINT('',(4.87558269014984,-2.,81.777182719677));
#9634=CARTESIAN_POINT('Origin',(5.11429163215176E-16,-2.,86.8));
#9635=CARTESIAN_POINT('',(-4.20530738557349,-2.,81.2039844717119));
#9636=CARTESIAN_POINT('Origin',(-24.6103750011395,-2.,69.1043082562094));
#9637=CARTESIAN_POINT('',(0.,0.,0.));
#9638=CARTESIAN_POINT('Origin',(-1.8,0.,0.));
#9639=CARTESIAN_POINT('',(-1.7,4.8,-5.8783046359073E-16));
#9640=CARTESIAN_POINT('Origin',(-1.7,1.83697019872105E-17,0.));
#9641=CARTESIAN_POINT('',(-1.955,4.8,-5.8783046359073E-16));
#9642=CARTESIAN_POINT('',(-1.8,4.8,-5.87830463590729E-16));
#9643=CARTESIAN_POINT('Origin',(-1.955,-2.84730380801758E-17,0.));
#9644=CARTESIAN_POINT('Origin',(-1.8,0.,0.));
#9645=CARTESIAN_POINT('',(1.7,4.872,-5.96647920544591E-16));
#9646=CARTESIAN_POINT('Origin',(1.7,6.42939569552361E-16,0.));
#9647=CARTESIAN_POINT('',(-1.7,4.872,-5.96647920544591E-16));
#9648=CARTESIAN_POINT('',(-1.8,4.872,-5.96647920544591E-16));
#9649=CARTESIAN_POINT('Origin',(-1.7,1.83697019872105E-17,0.));
#9650=CARTESIAN_POINT('Origin',(-1.8,0.,0.));
#9651=CARTESIAN_POINT('',(1.955,-4.8,5.90585918888811E-16));
#9652=CARTESIAN_POINT('',(1.955,4.8,-5.87830463590729E-16));
#9653=CARTESIAN_POINT('Origin',(1.955,6.89782309619747E-16,0.));
#9654=CARTESIAN_POINT('Origin',(1.955,6.89782309619747E-16,0.));
#9655=CARTESIAN_POINT('',(1.7,4.8,-5.87830463590729E-16));
#9656=CARTESIAN_POINT('',(-1.8,4.8,-5.87830463590729E-16));
#9657=CARTESIAN_POINT('Origin',(1.7,6.42939569552361E-16,0.));
#9658=CARTESIAN_POINT('Origin',(1.955,6.89782309619747E-16,0.));
#9659=CARTESIAN_POINT('',(2.,-4.845,-5.93341374186893E-16));
#9660=CARTESIAN_POINT('',(1.955,-4.8,-5.87830463590729E-16));
#9661=CARTESIAN_POINT('Origin',(2.,6.98048675513991E-16,0.));
#9662=CARTESIAN_POINT('Origin',(1.8,8.67361737988404E-16,0.));
#9663=CARTESIAN_POINT('',(1.8,6.,-7.34788079488412E-16));
#9664=CARTESIAN_POINT('Origin',(1.8,6.61309271539571E-16,0.));
#9665=CARTESIAN_POINT('',(2.,5.8,-7.10295143505465E-16));
#9666=CARTESIAN_POINT('Origin',(1.8,5.8,-7.10295143505465E-16));
#9667=CARTESIAN_POINT('Origin',(2.,6.98048675513991E-16,0.));
#9668=CARTESIAN_POINT('Origin',(-1.8,0.,0.));
#9669=CARTESIAN_POINT('',(-1.8,6.,-7.34788079488412E-16));
#9670=CARTESIAN_POINT('Origin',(-1.8,2.02467570659351E-31,0.));
#9671=CARTESIAN_POINT('',(-1.8,6.,-7.34788079488412E-16));
#9672=CARTESIAN_POINT('Origin',(-1.8,0.,0.));
#9673=CARTESIAN_POINT('',(-2.,5.8,-7.10295143505465E-16));
#9674=CARTESIAN_POINT('Origin',(-2.,-3.67394039744204E-17,0.));
#9675=CARTESIAN_POINT('Origin',(-1.8,5.8,-7.10295143505465E-16));
#9676=CARTESIAN_POINT('Origin',(-2.,-3.67394039744204E-17,0.));
#9677=CARTESIAN_POINT('',(-2.,4.845,-5.93341374186893E-16));
#9678=CARTESIAN_POINT('',(-2.,4.845,-5.93341374186893E-16));
#9679=CARTESIAN_POINT('Origin',(-2.,-3.67394039744204E-17,0.));
#9680=CARTESIAN_POINT('Origin',(-2.,5.8,0.));
#9681=CARTESIAN_POINT('Origin',(2.,5.8,0.));
#9682=CARTESIAN_POINT('Origin',(1.7,4.8,0.));
#9683=CARTESIAN_POINT('Origin',(-1.7,4.8,0.));
#9684=CARTESIAN_POINT('Origin',(-1.955,-2.84730380801757E-17,0.));
#9685=CARTESIAN_POINT('',(-1.955,3.1184375,3.81898450271607E-16));
#9686=CARTESIAN_POINT('',(-1.955,-3.1184375,-3.81898450271607E-16));
#9687=CARTESIAN_POINT('Origin',(-1.955,-2.84730380801757E-17,0.));
#9688=CARTESIAN_POINT('',(-2.,-3.0734375,-3.76387539675444E-16));
#9689=CARTESIAN_POINT('',(-1.955,-3.1184375,-3.81898450271607E-16));
#9690=CARTESIAN_POINT('Origin',(-2.,-3.67394039744204E-17,0.));
#9691=CARTESIAN_POINT('Origin',(-1.955,-2.84730380801757E-17,0.));
#9692=CARTESIAN_POINT('Origin',(-1.8,0.,0.));
#9693=CARTESIAN_POINT('',(-1.7890625,3.1184375,-3.81898450271607E-16));
#9694=CARTESIAN_POINT('',(-1.8,3.1184375,-3.81898450271607E-16));
#9695=CARTESIAN_POINT('Origin',(-1.7890625,2.00918615485137E-18,0.));
#9696=CARTESIAN_POINT('Origin',(-1.7890625,0.,0.));
#9697=CARTESIAN_POINT('',(-1.6625,3.2,-3.91886975727153E-16));
#9698=CARTESIAN_POINT('Origin',(-1.7890625,3.25741379310345,-3.98918137522258E-16));
#9699=CARTESIAN_POINT('Origin',(-1.6625,2.52583402324144E-17,0.));
#9700=CARTESIAN_POINT('Origin',(-1.8,0.,0.));
#9701=CARTESIAN_POINT('',(-1.6625,3.272,-4.00704432681014E-16));
#9702=CARTESIAN_POINT('Origin',(-1.6625,2.52583402324144E-17,0.));
#9703=CARTESIAN_POINT('',(1.6625,3.272,-4.00704432681014E-16));
#9704=CARTESIAN_POINT('',(-1.8,3.272,-4.00704432681014E-16));
#9705=CARTESIAN_POINT('Origin',(1.6625,6.36050931307157E-16,0.));
#9706=CARTESIAN_POINT('Origin',(1.7890625,8.67361737988404E-16,0.));
#9707=CARTESIAN_POINT('',(1.6625,3.2,-3.91886975727153E-16));
#9708=CARTESIAN_POINT('Origin',(1.6625,6.36050931307157E-16,0.));
#9709=CARTESIAN_POINT('',(1.7890625,3.1184375,-3.81898450271607E-16));
#9710=CARTESIAN_POINT('Origin',(1.7890625,3.25741379310345,-3.98918137522258E-16));
#9711=CARTESIAN_POINT('Origin',(1.7890625,6.5930008538472E-16,0.));
#9712=CARTESIAN_POINT('Origin',(-1.8,0.,0.));
#9713=CARTESIAN_POINT('',(1.955,3.1184375,-3.81898450271607E-16));
#9714=CARTESIAN_POINT('',(-1.8,3.1184375,-3.81898450271607E-16));
#9715=CARTESIAN_POINT('Origin',(1.955,6.89782309619747E-16,0.));
#9716=CARTESIAN_POINT('Origin',(2.,6.98048675513991E-16,0.));
#9717=CARTESIAN_POINT('',(2.,3.0734375,-3.76387539675444E-16));
#9718=CARTESIAN_POINT('',(2.,3.0734375,-3.76387539675444E-16));
#9719=CARTESIAN_POINT('Origin',(2.,6.98048675513991E-16,0.));
#9720=CARTESIAN_POINT('Origin',(1.8,8.67361737988404E-16,0.));
#9721=CARTESIAN_POINT('',(2.,2.2,-2.69422295812418E-16));
#9722=CARTESIAN_POINT('Origin',(2.,6.98048675513991E-16,0.));
#9723=CARTESIAN_POINT('',(1.8,2.,-2.44929359829471E-16));
#9724=CARTESIAN_POINT('Origin',(1.8,2.2,-2.69422295812418E-16));
#9725=CARTESIAN_POINT('Origin',(1.8,6.61309271539571E-16,0.));
#9726=CARTESIAN_POINT('Origin',(-1.8,0.,0.));
#9727=CARTESIAN_POINT('',(-1.8,2.,-2.44929359829471E-16));
#9728=CARTESIAN_POINT('',(-1.8,2.,-2.44929359829471E-16));
#9729=CARTESIAN_POINT('Origin',(-1.8,1.86988015034452E-31,0.));
#9730=CARTESIAN_POINT('Origin',(-1.8,0.,0.));
#9731=CARTESIAN_POINT('',(-2.,2.2,-2.69422295812418E-16));
#9732=CARTESIAN_POINT('Origin',(-1.8,2.2,-2.69422295812418E-16));
#9733=CARTESIAN_POINT('Origin',(-2.,-3.67394039744205E-17,0.));
#9734=CARTESIAN_POINT('Origin',(2.,2.2,0.));
#9735=CARTESIAN_POINT('Origin',(1.6625,3.272,0.));
#9736=CARTESIAN_POINT('Origin',(-1.6625,3.2,0.));
#9737=CARTESIAN_POINT('Origin',(-2.,2.2,0.));
#9738=CARTESIAN_POINT('Origin',(-1.8,0.,0.));
#9739=CARTESIAN_POINT('',(1.95,3.2,-3.91886975727153E-16));
#9740=CARTESIAN_POINT('Origin',(1.95,6.88863824520387E-16,0.));
#9741=CARTESIAN_POINT('',(1.85,3.2,-3.91886975727153E-16));
#9742=CARTESIAN_POINT('',(-1.8,3.2,-3.91886975727153E-16));
#9743=CARTESIAN_POINT('Origin',(1.85,6.70494122533176E-16,0.));
#9744=CARTESIAN_POINT('Origin',(1.86,8.67361737988404E-16,0.));
#9745=CARTESIAN_POINT('',(1.905,4.22108058265378,-5.16933282449E-16));
#9746=CARTESIAN_POINT('Origin',(1.905,6.80597458626142E-16,0.));
#9747=CARTESIAN_POINT('',(1.95,4.14313829631318,-5.07388105300476E-16));
#9748=CARTESIAN_POINT('Origin',(1.86,4.14313829631318,-5.07388105300475E-16));
#9749=CARTESIAN_POINT('Origin',(1.95,6.88863824520387E-16,0.));
#9750=CARTESIAN_POINT('Origin',(1.65333333333334,6.34367041958329E-16,0.));
#9751=CARTESIAN_POINT('',(1.65333333333334,4.36638040039984,-5.3472737812094E-16));
#9752=CARTESIAN_POINT('Origin',(1.65333333333334,6.34367041958329E-16,0.));
#9753=CARTESIAN_POINT('',(1.65333333333334,4.36638040039984,-5.3472737812094E-16));
#9754=CARTESIAN_POINT('Origin',(1.66333333333334,8.67361737988404E-16,0.));
#9755=CARTESIAN_POINT('',(1.64333333333333,4.38370090847553,-5.3684852859839E-16));
#9756=CARTESIAN_POINT('Origin',(1.64333333333334,6.32530071759608E-16,0.));
#9757=CARTESIAN_POINT('Origin',(1.66333333333334,4.38370090847553,-5.3684852859839E-16));
#9758=CARTESIAN_POINT('Origin',(1.76333333333333,8.67361737988404E-16,0.));
#9759=CARTESIAN_POINT('',(1.86725638178747,4.64,-5.68236114804372E-16));
#9760=CARTESIAN_POINT('Origin',(1.86725638178747,6.73664068441309E-16,0.));
#9761=CARTESIAN_POINT('',(1.64333333333333,4.58,-5.60888234009488E-16));
#9762=CARTESIAN_POINT('Origin',(1.76333333333333,4.58,-5.60888234009488E-16));
#9763=CARTESIAN_POINT('Origin',(1.64333333333334,6.32530071759608E-16,0.));
#9764=CARTESIAN_POINT('Origin',(1.90725638178747,6.81011949236193E-16,0.));
#9765=CARTESIAN_POINT('',(1.90725638178747,4.57071796769724,-5.59751512894572E-16));
#9766=CARTESIAN_POINT('Origin',(1.90725638178747,6.81011949236193E-16,0.));
#9767=CARTESIAN_POINT('',(1.90725638178747,4.57071796769724,-5.59751512894572E-16));
#9768=CARTESIAN_POINT('Origin',(1.80333333333334,8.67361737988404E-16,0.));
#9769=CARTESIAN_POINT('',(1.80333333333334,4.39071796769724,-5.3770787050992E-16));
#9770=CARTESIAN_POINT('Origin',(1.80333333333334,6.61921594939145E-16,0.));
#9771=CARTESIAN_POINT('Origin',(1.80333333333334,4.51071796769724,-5.52403632099688E-16));
#9772=CARTESIAN_POINT('Origin',(1.80333333333334,8.67361737988404E-16,0.));
#9773=CARTESIAN_POINT('',(1.99385892216591,4.62071796769724,-5.65874746890309E-16));
#9774=CARTESIAN_POINT('Origin',(1.99385892216591,6.96920577817067E-16,0.));
#9775=CARTESIAN_POINT('',(1.80333333333334,4.29071796769724,-5.25461402518447E-16));
#9776=CARTESIAN_POINT('Origin',(1.80333333333334,4.51071796769724,-5.52403632099688E-16));
#9777=CARTESIAN_POINT('Origin',(1.80333333333334,6.61921594939145E-16,0.));
#9778=CARTESIAN_POINT('Origin',(1.99385892216591,6.96920577817067E-16,0.));
#9779=CARTESIAN_POINT('',(1.95385892216591,4.69,-5.74359348800109E-16));
#9780=CARTESIAN_POINT('Origin',(1.95385892216591,6.89572697022182E-16,0.));
#9781=CARTESIAN_POINT('',(1.99385892216591,4.62071796769724,-5.65874746890309E-16));
#9782=CARTESIAN_POINT('Origin',(1.76333333333333,8.67361737988404E-16,0.));
#9783=CARTESIAN_POINT('',(1.54333333333334,4.58,-5.60888234009488E-16));
#9784=CARTESIAN_POINT('Origin',(1.54333333333334,6.14160369772398E-16,0.));
#9785=CARTESIAN_POINT('Origin',(1.76333333333333,4.58,-5.60888234009488E-16));
#9786=CARTESIAN_POINT('Origin',(1.66333333333334,8.67361737988404E-16,0.));
#9787=CARTESIAN_POINT('',(1.60333333333334,4.27977786002139,-5.24121625733691E-16));
#9788=CARTESIAN_POINT('Origin',(1.60333333333334,6.25182190964724E-16,0.));
#9789=CARTESIAN_POINT('',(1.54333333333333,4.38370090847553,-5.3684852859839E-16));
#9790=CARTESIAN_POINT('Origin',(1.66333333333334,4.38370090847553,-5.3684852859839E-16));
#9791=CARTESIAN_POINT('Origin',(1.54333333333334,6.14160369772398E-16,0.));
#9792=CARTESIAN_POINT('Origin',(1.60333333333334,6.25182190964724E-16,0.));
#9793=CARTESIAN_POINT('',(1.85,4.13736479362129,-5.06681055141326E-16));
#9794=CARTESIAN_POINT('Origin',(1.85,6.70494122533176E-16,0.));
#9795=CARTESIAN_POINT('',(1.60333333333334,4.27977786002139,-5.2412162573369E-16));
#9796=CARTESIAN_POINT('Origin',(1.85,4.14313829631318,0.));
#9797=CARTESIAN_POINT('Origin',(1.54333333333334,4.58,0.));
#9798=CARTESIAN_POINT('Origin',(1.80333333333334,4.29071796769724,0.));
#9799=CARTESIAN_POINT('Origin',(1.64333333333334,4.58,0.));
#9800=CARTESIAN_POINT('Origin',(1.95,4.14313829631318,0.));
#9801=CARTESIAN_POINT('Origin',(1.8,0.,0.));
#9802=CARTESIAN_POINT('',(-1.95,3.2,3.91886975727153E-16));
#9803=CARTESIAN_POINT('Origin',(-1.95,6.88863824520387E-16,0.));
#9804=CARTESIAN_POINT('',(-1.85,3.2,3.91886975727153E-16));
#9805=CARTESIAN_POINT('',(1.8,3.2,3.91886975727153E-16));
#9806=CARTESIAN_POINT('Origin',(-1.85,6.70494122533176E-16,0.));
#9807=CARTESIAN_POINT('Origin',(-1.86,8.67361737988404E-16,0.));
#9808=CARTESIAN_POINT('',(-1.905,4.22108058265378,5.16933282449E-16));
#9809=CARTESIAN_POINT('Origin',(-1.905,6.80597458626142E-16,0.));
#9810=CARTESIAN_POINT('',(-1.95,4.14313829631318,5.07388105300476E-16));
#9811=CARTESIAN_POINT('Origin',(-1.86,4.14313829631318,5.07388105300475E-16));
#9812=CARTESIAN_POINT('Origin',(-1.95,6.88863824520387E-16,0.));
#9813=CARTESIAN_POINT('Origin',(-1.65333333333334,6.34367041958329E-16,
0.));
#9814=CARTESIAN_POINT('',(-1.65333333333334,4.36638040039984,5.3472737812094E-16));
#9815=CARTESIAN_POINT('Origin',(-1.65333333333334,6.34367041958329E-16,
0.));
#9816=CARTESIAN_POINT('',(-1.65333333333334,4.36638040039984,5.3472737812094E-16));
#9817=CARTESIAN_POINT('Origin',(-1.66333333333334,8.67361737988404E-16,
0.));
#9818=CARTESIAN_POINT('',(-1.64333333333333,4.38370090847553,5.3684852859839E-16));
#9819=CARTESIAN_POINT('Origin',(-1.64333333333334,6.32530071759608E-16,
0.));
#9820=CARTESIAN_POINT('Origin',(-1.66333333333334,4.38370090847553,5.3684852859839E-16));
#9821=CARTESIAN_POINT('Origin',(-1.76333333333333,8.67361737988404E-16,
0.));
#9822=CARTESIAN_POINT('',(-1.86725638178747,4.64,5.68236114804372E-16));
#9823=CARTESIAN_POINT('Origin',(-1.86725638178747,6.73664068441309E-16,
0.));
#9824=CARTESIAN_POINT('',(-1.64333333333333,4.58,5.60888234009488E-16));
#9825=CARTESIAN_POINT('Origin',(-1.76333333333333,4.58,5.60888234009488E-16));
#9826=CARTESIAN_POINT('Origin',(-1.64333333333334,6.32530071759608E-16,
0.));
#9827=CARTESIAN_POINT('Origin',(-1.90725638178747,6.81011949236193E-16,
0.));
#9828=CARTESIAN_POINT('',(-1.90725638178747,4.57071796769724,5.59751512894572E-16));
#9829=CARTESIAN_POINT('Origin',(-1.90725638178747,6.81011949236193E-16,
0.));
#9830=CARTESIAN_POINT('',(-1.90725638178747,4.57071796769724,5.59751512894572E-16));
#9831=CARTESIAN_POINT('Origin',(-1.80333333333334,8.67361737988404E-16,
0.));
#9832=CARTESIAN_POINT('',(-1.80333333333334,4.39071796769724,5.3770787050992E-16));
#9833=CARTESIAN_POINT('Origin',(-1.80333333333334,6.61921594939145E-16,
0.));
#9834=CARTESIAN_POINT('Origin',(-1.80333333333334,4.51071796769724,5.52403632099688E-16));
#9835=CARTESIAN_POINT('Origin',(-1.80333333333334,8.67361737988404E-16,
0.));
#9836=CARTESIAN_POINT('',(-1.99385892216591,4.62071796769724,5.65874746890309E-16));
#9837=CARTESIAN_POINT('Origin',(-1.99385892216591,6.96920577817067E-16,
0.));
#9838=CARTESIAN_POINT('',(-1.80333333333334,4.29071796769724,5.25461402518447E-16));
#9839=CARTESIAN_POINT('Origin',(-1.80333333333334,4.51071796769724,5.52403632099688E-16));
#9840=CARTESIAN_POINT('Origin',(-1.80333333333334,6.61921594939145E-16,
0.));
#9841=CARTESIAN_POINT('Origin',(-1.99385892216591,6.96920577817067E-16,
0.));
#9842=CARTESIAN_POINT('',(-1.95385892216591,4.69,5.74359348800109E-16));
#9843=CARTESIAN_POINT('Origin',(-1.95385892216591,6.89572697022182E-16,
0.));
#9844=CARTESIAN_POINT('',(-1.99385892216591,4.62071796769724,5.65874746890309E-16));
#9845=CARTESIAN_POINT('Origin',(-1.76333333333333,8.67361737988404E-16,
0.));
#9846=CARTESIAN_POINT('',(-1.54333333333334,4.58,5.60888234009488E-16));
#9847=CARTESIAN_POINT('Origin',(-1.54333333333334,6.14160369772398E-16,
0.));
#9848=CARTESIAN_POINT('Origin',(-1.76333333333333,4.58,5.60888234009488E-16));
#9849=CARTESIAN_POINT('Origin',(-1.66333333333334,8.67361737988404E-16,
0.));
#9850=CARTESIAN_POINT('',(-1.60333333333334,4.27977786002139,5.24121625733691E-16));
#9851=CARTESIAN_POINT('Origin',(-1.60333333333334,6.25182190964724E-16,
0.));
#9852=CARTESIAN_POINT('',(-1.54333333333333,4.38370090847553,5.3684852859839E-16));
#9853=CARTESIAN_POINT('Origin',(-1.66333333333334,4.38370090847553,5.3684852859839E-16));
#9854=CARTESIAN_POINT('Origin',(-1.54333333333334,6.14160369772398E-16,
0.));
#9855=CARTESIAN_POINT('Origin',(-1.60333333333334,6.25182190964724E-16,
0.));
#9856=CARTESIAN_POINT('',(-1.85,4.13736479362129,5.06681055141326E-16));
#9857=CARTESIAN_POINT('Origin',(-1.85,6.70494122533176E-16,0.));
#9858=CARTESIAN_POINT('',(-1.60333333333334,4.27977786002139,5.2412162573369E-16));
#9859=CARTESIAN_POINT('Origin',(-1.85,4.14313829631318,0.));
#9860=CARTESIAN_POINT('Origin',(-1.54333333333334,4.58,0.));
#9861=CARTESIAN_POINT('Origin',(-1.80333333333334,4.29071796769724,0.));
#9862=CARTESIAN_POINT('Origin',(-1.64333333333334,4.58,0.));
#9863=CARTESIAN_POINT('Origin',(-1.95,4.14313829631318,0.));
#9864=CARTESIAN_POINT('',(-1.66533453693773E-16,-2.,86.8));
#9865=CARTESIAN_POINT('',(3.64981768126446E-16,-4.00000000000001,42.));
#9866=CARTESIAN_POINT('',(0.,0.,0.));
#9867=CARTESIAN_POINT('',(0.,0.,0.));
#9868=CARTESIAN_POINT('',(0.,0.,0.));
#9869=CARTESIAN_POINT('',(0.,0.,0.));
#9870=CARTESIAN_POINT('',(0.,0.,0.));
#9871=CARTESIAN_POINT('',(4.02519227649757E-16,-2.,42.));
#9872=UNCERTAINTY_MEASURE_WITH_UNIT(LENGTH_MEASURE(0.01),#9892,
'DISTANCE_ACCURACY_VALUE',
'Maximum model space distance between geometric entities at asserted c
onnectivities');
#9873=UNCERTAINTY_MEASURE_WITH_UNIT(LENGTH_MEASURE(0.01),#9892,
'DISTANCE_ACCURACY_VALUE',
'Maximum model space distance between geometric entities at asserted c
onnectivities');
#9874=UNCERTAINTY_MEASURE_WITH_UNIT(LENGTH_MEASURE(0.01),#9892,
'DISTANCE_ACCURACY_VALUE',
'Maximum model space distance between geometric entities at asserted c
onnectivities');
#9875=UNCERTAINTY_MEASURE_WITH_UNIT(LENGTH_MEASURE(0.01),#9892,
'DISTANCE_ACCURACY_VALUE',
'Maximum model space distance between geometric entities at asserted c
onnectivities');
#9876=UNCERTAINTY_MEASURE_WITH_UNIT(LENGTH_MEASURE(0.01),#9892,
'DISTANCE_ACCURACY_VALUE',
'Maximum model space distance between geometric entities at asserted c
onnectivities');
#9877=UNCERTAINTY_MEASURE_WITH_UNIT(LENGTH_MEASURE(0.01),#9892,
'DISTANCE_ACCURACY_VALUE',
'Maximum model space distance between geometric entities at asserted c
onnectivities');
#9878=UNCERTAINTY_MEASURE_WITH_UNIT(LENGTH_MEASURE(0.01),#9892,
'DISTANCE_ACCURACY_VALUE',
'Maximum model space distance between geometric entities at asserted c
onnectivities');
#9879=UNCERTAINTY_MEASURE_WITH_UNIT(LENGTH_MEASURE(0.01),#9892,
'DISTANCE_ACCURACY_VALUE',
'Maximum model space distance between geometric entities at asserted c
onnectivities');
#9880=UNCERTAINTY_MEASURE_WITH_UNIT(LENGTH_MEASURE(0.01),#9892,
'DISTANCE_ACCURACY_VALUE',
'Maximum model space distance between geometric entities at asserted c
onnectivities');
#9881=UNCERTAINTY_MEASURE_WITH_UNIT(LENGTH_MEASURE(0.01),#9892,
'DISTANCE_ACCURACY_VALUE',
'Maximum model space distance between geometric entities at asserted c
onnectivities');
#9882=(
GEOMETRIC_REPRESENTATION_CONTEXT(3)
GLOBAL_UNCERTAINTY_ASSIGNED_CONTEXT((#9872))
GLOBAL_UNIT_ASSIGNED_CONTEXT((#9892,#9894,#9895))
REPRESENTATION_CONTEXT('','3D')
);
#9883=(
GEOMETRIC_REPRESENTATION_CONTEXT(3)
GLOBAL_UNCERTAINTY_ASSIGNED_CONTEXT((#9873))
GLOBAL_UNIT_ASSIGNED_CONTEXT((#9892,#9894,#9895))
REPRESENTATION_CONTEXT('','3D')
);
#9884=(
GEOMETRIC_REPRESENTATION_CONTEXT(3)
GLOBAL_UNCERTAINTY_ASSIGNED_CONTEXT((#9874))
GLOBAL_UNIT_ASSIGNED_CONTEXT((#9892,#9894,#9895))
REPRESENTATION_CONTEXT('','3D')
);
#9885=(
GEOMETRIC_REPRESENTATION_CONTEXT(3)
GLOBAL_UNCERTAINTY_ASSIGNED_CONTEXT((#9875))
GLOBAL_UNIT_ASSIGNED_CONTEXT((#9892,#9894,#9895))
REPRESENTATION_CONTEXT('','3D')
);
#9886=(
GEOMETRIC_REPRESENTATION_CONTEXT(3)
GLOBAL_UNCERTAINTY_ASSIGNED_CONTEXT((#9876))
GLOBAL_UNIT_ASSIGNED_CONTEXT((#9892,#9894,#9895))
REPRESENTATION_CONTEXT('','3D')
);
#9887=(
GEOMETRIC_REPRESENTATION_CONTEXT(3)
GLOBAL_UNCERTAINTY_ASSIGNED_CONTEXT((#9877))
GLOBAL_UNIT_ASSIGNED_CONTEXT((#9892,#9894,#9895))
REPRESENTATION_CONTEXT('','3D')
);
#9888=(
GEOMETRIC_REPRESENTATION_CONTEXT(3)
GLOBAL_UNCERTAINTY_ASSIGNED_CONTEXT((#9878))
GLOBAL_UNIT_ASSIGNED_CONTEXT((#9892,#9894,#9895))
REPRESENTATION_CONTEXT('','3D')
);
#9889=(
GEOMETRIC_REPRESENTATION_CONTEXT(3)
GLOBAL_UNCERTAINTY_ASSIGNED_CONTEXT((#9879))
GLOBAL_UNIT_ASSIGNED_CONTEXT((#9892,#9894,#9895))
REPRESENTATION_CONTEXT('','3D')
);
#9890=(
GEOMETRIC_REPRESENTATION_CONTEXT(3)
GLOBAL_UNCERTAINTY_ASSIGNED_CONTEXT((#9880))
GLOBAL_UNIT_ASSIGNED_CONTEXT((#9892,#9894,#9895))
REPRESENTATION_CONTEXT('','3D')
);
#9891=(
GEOMETRIC_REPRESENTATION_CONTEXT(3)
GLOBAL_UNCERTAINTY_ASSIGNED_CONTEXT((#9881))
GLOBAL_UNIT_ASSIGNED_CONTEXT((#9892,#9894,#9895))
REPRESENTATION_CONTEXT('','3D')
);
#9892=(
LENGTH_UNIT()
NAMED_UNIT(*)
SI_UNIT(.MILLI.,.METRE.)
);
#9893=(
LENGTH_UNIT()
NAMED_UNIT(*)
SI_UNIT($,.METRE.)
);
#9894=(
NAMED_UNIT(*)
PLANE_ANGLE_UNIT()
SI_UNIT($,.RADIAN.)
);
#9895=(
NAMED_UNIT(*)
SI_UNIT($,.STERADIAN.)
SOLID_ANGLE_UNIT()
);
#9896=SHAPE_DEFINITION_REPRESENTATION(#9905,#9922);
#9897=SHAPE_DEFINITION_REPRESENTATION(#9906,#9923);
#9898=SHAPE_DEFINITION_REPRESENTATION(#9907,#9924);
#9899=SHAPE_DEFINITION_REPRESENTATION(#9908,#9925);
#9900=SHAPE_DEFINITION_REPRESENTATION(#9909,#9926);
#9901=SHAPE_DEFINITION_REPRESENTATION(#9910,#9927);
#9902=SHAPE_DEFINITION_REPRESENTATION(#9911,#9928);
#9903=SHAPE_DEFINITION_REPRESENTATION(#9912,#9929);
#9904=SHAPE_DEFINITION_REPRESENTATION(#9913,#9930);
#9905=PRODUCT_DEFINITION_SHAPE('',$,#9932);
#9906=PRODUCT_DEFINITION_SHAPE('',$,#9933);
#9907=PRODUCT_DEFINITION_SHAPE('',$,#9934);
#9908=PRODUCT_DEFINITION_SHAPE('',$,#9935);
#9909=PRODUCT_DEFINITION_SHAPE('',$,#9936);
#9910=PRODUCT_DEFINITION_SHAPE('',$,#9937);
#9911=PRODUCT_DEFINITION_SHAPE('',$,#9938);
#9912=PRODUCT_DEFINITION_SHAPE('',$,#9939);
#9913=PRODUCT_DEFINITION_SHAPE('',$,#9940);
#9914=PRODUCT_DEFINITION_SHAPE($,$,#35);
#9915=PRODUCT_DEFINITION_SHAPE($,$,#36);
#9916=PRODUCT_DEFINITION_SHAPE($,$,#37);
#9917=PRODUCT_DEFINITION_SHAPE($,$,#38);
#9918=PRODUCT_DEFINITION_SHAPE($,$,#39);
#9919=PRODUCT_DEFINITION_SHAPE($,$,#40);
#9920=PRODUCT_DEFINITION_SHAPE($,$,#41);
#9921=PRODUCT_DEFINITION_SHAPE($,$,#42);
#9922=SHAPE_REPRESENTATION('',(#5719,#6363,#6364,#6365,#6366,#6367,#6368,
#6369,#6370),#9882);
#9923=SHAPE_REPRESENTATION('',(#5720),#9883);
#9924=SHAPE_REPRESENTATION('',(#5863),#9884);
#9925=SHAPE_REPRESENTATION('',(#5890),#9885);
#9926=SHAPE_REPRESENTATION('',(#5919),#9886);
#9927=SHAPE_REPRESENTATION('',(#5928),#9887);
#9928=SHAPE_REPRESENTATION('',(#5948),#9888);
#9929=SHAPE_REPRESENTATION('',(#6182),#9889);
#9930=SHAPE_REPRESENTATION('',(#6220),#9890);
#9931=PRODUCT_DEFINITION_CONTEXT('part definition',#9960,'design');
#9932=PRODUCT_DEFINITION('BR-059','BR-059',#9941,#9931);
#9933=PRODUCT_DEFINITION(
'7804K102_Corrosion-Resistant 440C Stainless Steel Ball Bearing',
'Bearing_01',#9942,#9931);
#9934=PRODUCT_DEFINITION('SPHS BS 4183 - M4 x 6 Steel 4.6 Plain',
'Screw',#9943,#9931);
#9935=PRODUCT_DEFINITION('base','Base',#9944,#9931);
#9936=PRODUCT_DEFINITION('spacer','Spacer',#9945,#9931);
#9937=PRODUCT_DEFINITION('Pin','Pin',#9946,#9931);
#9938=PRODUCT_DEFINITION('Wheel','Wheel',#9947,#9931);
#9939=PRODUCT_DEFINITION('Arm','Arm',#9948,#9931);
#9940=PRODUCT_DEFINITION(
'7804K102_Corrosion-Resistant 440C Stainless Steel Ball Bearing_1',
'Bearing_02',#9949,#9931);
#9941=PRODUCT_DEFINITION_FORMATION('',$,#9962);
#9942=PRODUCT_DEFINITION_FORMATION('',$,#9963);
#9943=PRODUCT_DEFINITION_FORMATION('',$,#9964);
#9944=PRODUCT_DEFINITION_FORMATION('',$,#9965);
#9945=PRODUCT_DEFINITION_FORMATION('',$,#9966);
#9946=PRODUCT_DEFINITION_FORMATION('',$,#9967);
#9947=PRODUCT_DEFINITION_FORMATION('',$,#9968);
#9948=PRODUCT_DEFINITION_FORMATION('',$,#9969);
#9949=PRODUCT_DEFINITION_FORMATION('',$,#9970);
#9950=PRODUCT_RELATED_PRODUCT_CATEGORY('BR-059','BR-059',(#9962));
#9951=PRODUCT_RELATED_PRODUCT_CATEGORY('Bearing_01','Bearing_01',(#9963));
#9952=PRODUCT_RELATED_PRODUCT_CATEGORY('Screw','Screw',(#9964));
#9953=PRODUCT_RELATED_PRODUCT_CATEGORY('Base','Base',(#9965));
#9954=PRODUCT_RELATED_PRODUCT_CATEGORY('Spacer','Spacer',(#9966));
#9955=PRODUCT_RELATED_PRODUCT_CATEGORY('Pin','Pin',(#9967));
#9956=PRODUCT_RELATED_PRODUCT_CATEGORY('Wheel','Wheel',(#9968));
#9957=PRODUCT_RELATED_PRODUCT_CATEGORY('Arm','Arm',(#9969));
#9958=PRODUCT_RELATED_PRODUCT_CATEGORY('Bearing_02','Bearing_02',(#9970));
#9959=APPLICATION_PROTOCOL_DEFINITION('international standard',
'automotive_design',2009,#9960);
#9960=APPLICATION_CONTEXT(
'Core Data for Automotive Mechanical Design Process');
#9961=PRODUCT_CONTEXT('part definition',#9960,'mechanical');
#9962=PRODUCT('BR-059','BR-059',$,(#9961));
#9963=PRODUCT(
'7804K102_Corrosion-Resistant 440C Stainless Steel Ball Bearing',
'Bearing_01',$,(#9961));
#9964=PRODUCT('SPHS BS 4183 - M4 x 6 Steel 4.6 Plain','Screw',
'Slotted Pan Head Screw BS 4183 - M4 x 6',(#9961));
#9965=PRODUCT('base','Base',$,(#9961));
#9966=PRODUCT('spacer','Spacer',$,(#9961));
#9967=PRODUCT('Pin','Pin',$,(#9961));
#9968=PRODUCT('Wheel','Wheel',$,(#9961));
#9969=PRODUCT('Arm','Arm',$,(#9961));
#9970=PRODUCT(
'7804K102_Corrosion-Resistant 440C Stainless Steel Ball Bearing_1',
'Bearing_02',$,(#9961));
#9971=PRESENTATION_STYLE_ASSIGNMENT((#9976));
#9972=PRESENTATION_STYLE_ASSIGNMENT((#9977));
#9973=PRESENTATION_STYLE_ASSIGNMENT((#9978));
#9974=PRESENTATION_STYLE_ASSIGNMENT((#9979));
#9975=PRESENTATION_STYLE_ASSIGNMENT((#9980));
#9976=SURFACE_STYLE_USAGE(.BOTH.,#9981);
#9977=SURFACE_STYLE_USAGE(.BOTH.,#9982);
#9978=SURFACE_STYLE_USAGE(.BOTH.,#9983);
#9979=SURFACE_STYLE_USAGE(.BOTH.,#9984);
#9980=SURFACE_STYLE_USAGE(.BOTH.,#9985);
#9981=SURFACE_SIDE_STYLE('',(#9986));
#9982=SURFACE_SIDE_STYLE('',(#9987));
#9983=SURFACE_SIDE_STYLE('',(#9988));
#9984=SURFACE_SIDE_STYLE('',(#9989));
#9985=SURFACE_SIDE_STYLE('',(#9990));
#9986=SURFACE_STYLE_FILL_AREA(#9991);
#9987=SURFACE_STYLE_FILL_AREA(#9992);
#9988=SURFACE_STYLE_FILL_AREA(#9993);
#9989=SURFACE_STYLE_FILL_AREA(#9994);
#9990=SURFACE_STYLE_FILL_AREA(#9995);
#9991=FILL_AREA_STYLE('Steel - Satin',(#9996));
#9992=FILL_AREA_STYLE('Opaque(160,160,160)',(#9997));
#9993=FILL_AREA_STYLE('Opaque(48,59,150)',(#9998));
#9994=FILL_AREA_STYLE('Opaque(255,242,183)',(#9999));
#9995=FILL_AREA_STYLE('Opaque(203,203,203)',(#10000));
#9996=FILL_AREA_STYLE_COLOUR('Steel - Satin',#10001);
#9997=FILL_AREA_STYLE_COLOUR('Opaque(160,160,160)',#10002);
#9998=FILL_AREA_STYLE_COLOUR('Opaque(48,59,150)',#10003);
#9999=FILL_AREA_STYLE_COLOUR('Opaque(255,242,183)',#10004);
#10000=FILL_AREA_STYLE_COLOUR('Opaque(203,203,203)',#10005);
#10001=COLOUR_RGB('Steel - Satin', 0.09019608, 0.27058824, 0.51372549);
#10002=COLOUR_RGB('Opaque(160,160,160)', 0.09019608, 0.27058824, 0.51372549);
#10003=COLOUR_RGB('Opaque(48,59,150)', 0.72549020, 0.75294118, 0.79215686);
#10004=COLOUR_RGB('Opaque(255,242,183)', 0.08235294, 0.09019608, 0.10196078);
#10005=COLOUR_RGB('Opaque(203,203,203)', 0.40784314, 0.44705882, 0.49803922);
ENDSEC;
END-ISO-10303-21;
